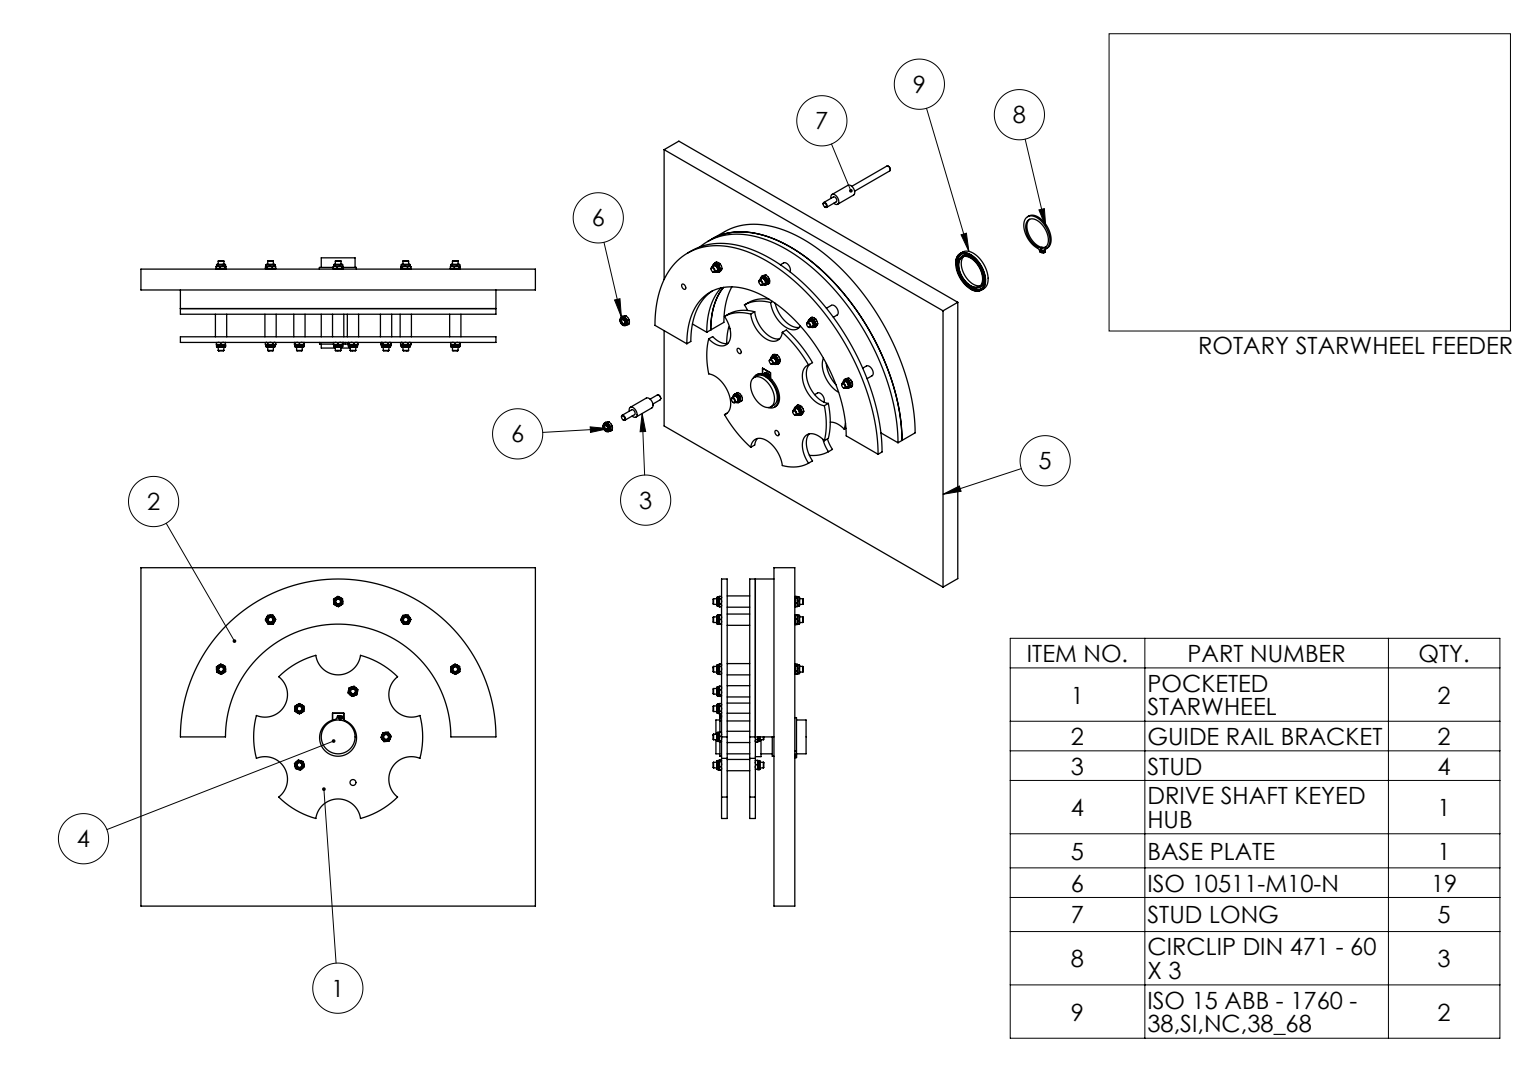
ISO-10303-21;
HEADER;
FILE_DESCRIPTION (('STEP AP214'),
    '1' );
FILE_NAME ('MAS-196',
    '2026-10-23T05:12:30',
    ( '' ),
    ( '' ),
    'SwSTEP 2.0',
    'SolidWorks 2026',
    '' );
FILE_SCHEMA (( 'AUTOMOTIVE_DESIGN' ));
ENDSEC;

DATA;
#1 = LINE ( 'NONE', #2495, #1142 ) ;
#2 = SURFACE_SIDE_STYLE ('',( #1097 ) ) ;
#3 = SURFACE_STYLE_USAGE ( .BOTH. , #3079 ) ;
#4 = AXIS2_PLACEMENT_3D ( 'NONE', #5314, #2448, #2411 ) ;
#5 = CARTESIAN_POINT ( 'NONE',  ( -63.76644452187071721, 49.96174644486006855, -40.00000000000000000 ) ) ;
#6 = PRODUCT ( 'Pocketed Starwheel', 'Pocketed Starwheel', '', ( #881 ) ) ;
#7 = ORIENTED_EDGE ( 'NONE', *, *, #982, .F. ) ;
#8 = EDGE_LOOP ( 'NONE', ( #780, #5698, #1230, #898 ) ) ;
#9 = AXIS2_PLACEMENT_3D ( 'NONE', #5192, #2676, #2095 ) ;
#10 = CARTESIAN_POINT ( 'NONE',  ( 213.0929183184020701, 119.9981648402868331, 10.00000000000000000 ) ) ;
#11 = CARTESIAN_POINT ( 'NONE',  ( 5.459126460941067016, -34.89491303563345070, -3.000000000000000000 ) ) ;
#12 = CIRCLE ( 'NONE', #1262, 6.099504629071905271 ) ;
#13 = CARTESIAN_POINT ( 'NONE',  ( 3.199999999999996181, 4.555686092828153507E-15, 37.19999999999999574 ) ) ;
#14 = ORIENTED_EDGE ( 'NONE', *, *, #6597, .T. ) ;
#15 = ORIENTED_EDGE ( 'NONE', *, *, #7014, .T. ) ;
#16 = AXIS2_PLACEMENT_3D ( 'NONE', #1817, #35, #4883 ) ;
#17 = DIRECTION ( 'NONE',  ( 1.000000000000000000, 0.000000000000000000, 0.000000000000000000 ) ) ;
#18 = CARTESIAN_POINT ( 'NONE',  ( -5.249999999999968026, 239.9963296805737230, 10.00000000000000000 ) ) ;
#19 = FACE_OUTER_BOUND ( 'NONE', #6377, .T. ) ;
#20 = DIRECTION ( 'NONE',  ( -1.000000000000000000, 0.000000000000000000, 0.000000000000000000 ) ) ;
#21 = CARTESIAN_POINT ( 'NONE',  ( -279.9963296805736945, 3.428966089163216048E-14, 0.000000000000000000 ) ) ;
#22 = ORIENTED_EDGE ( 'NONE', *, *, #2120, .F. ) ;
#23 = AXIS2_PLACEMENT_3D ( 'NONE', #6138, #4316, #7358 ) ;
#24 = CARTESIAN_POINT ( 'NONE',  ( 129.9038105676649764, 75.00000000000153477, 10.00000000000000000 ) ) ;
#25 = DIRECTION ( 'NONE',  ( -0.000000000000000000, -0.000000000000000000, 1.000000000000000000 ) ) ;
#26 = DIRECTION ( 'NONE',  ( -0.000000000000000000, -0.000000000000000000, 1.000000000000000000 ) ) ;
#27 = CARTESIAN_POINT ( 'NONE',  ( -7.039801714450301422E-15, 0.000000000000000000, -82.99999999999995737 ) ) ;
#28 = CARTESIAN_POINT ( 'NONE',  ( -58.76644452187068168, 49.96174644486002592, -40.00000000000000000 ) ) ;
#29 = DIRECTION ( 'NONE',  ( -1.000000000000000000, 0.000000000000000000, 0.000000000000000000 ) ) ;
#30 = ORIENTED_EDGE ( 'NONE', *, *, #1780, .F. ) ;
#31 = CIRCLE ( 'NONE', #2437, 40.00000000000001421 ) ;
#32 = EDGE_CURVE ( 'NONE', #3001, #1611, #576, .T. ) ;
#33 = ORIENTED_EDGE ( 'NONE', *, *, #894, .F. ) ;
#34 = ORIENTED_EDGE ( 'NONE', *, *, #1918, .F. ) ;
#35 = DIRECTION ( 'NONE',  ( -0.000000000000000000, -0.000000000000000000, 1.000000000000000000 ) ) ;
#36 =( NAMED_UNIT ( * ) PLANE_ANGLE_UNIT ( ) SI_UNIT ( $, .RADIAN. ) );
#37 = CIRCLE ( 'NONE', #2942, 5.249999999999991118 ) ;
#38 = PRODUCT_DEFINITION_FORMATION_WITH_SPECIFIED_SOURCE ( 'ANY', '', #6, .NOT_KNOWN. ) ;
#39 = DIRECTION ( 'NONE',  ( 1.000000000000000000, 0.000000000000000000, 0.000000000000000000 ) ) ;
#40 = ADVANCED_FACE ( 'NONE', ( #3233 ), #3303, .T. ) ;
#41 = ORIENTED_EDGE ( 'NONE', *, *, #4752, .T. ) ;
#42 = ORIENTED_EDGE ( 'NONE', *, *, #2330, .T. ) ;
#43 = CARTESIAN_POINT ( 'NONE',  ( -68.76644452187024115, -49.96174644486060856, 10.00000000000000000 ) ) ;
#44 = LINE ( 'NONE', #2388, #7655 ) ;
#45 = AXIS2_PLACEMENT_3D ( 'NONE', #3946, #5204, #2688 ) ;
#46 = DIRECTION ( 'NONE',  ( 0.000000000000000000, -1.000000000000000000, 0.000000000000000000 ) ) ;
#47 = VERTEX_POINT ( 'NONE', #965 ) ;
#48 = EDGE_CURVE ( 'NONE', #5972, #47, #4560, .T. ) ;
#49 = ORIENTED_EDGE ( 'NONE', *, *, #2998, .F. ) ;
#50 = COLOUR_RGB ( '',0.8941176470588234615, 0.8941176470588234615, 0.8941176470588234615 ) ;
#51 = DIRECTION ( 'NONE',  ( -0.000000000000000000, -0.000000000000000000, 1.000000000000000000 ) ) ;
#52 = CARTESIAN_POINT ( 'NONE',  ( 0.000000000000000000, 0.000000000000000000, 0.000000000000000000 ) ) ;
#53 = DIRECTION ( 'NONE',  ( 0.000000000000000000, 0.000000000000000000, -1.000000000000000000 ) ) ;
#54 = FACE_BOUND ( 'NONE', #7641, .T. ) ;
#55 = CONTEXT_DEPENDENT_SHAPE_REPRESENTATION ( #2402, #2599 ) ;
#56 = DIRECTION ( 'NONE',  ( 1.000000000000000000, 0.000000000000000000, 0.000000000000000000 ) ) ;
#57 = VERTEX_POINT ( 'NONE', #3381 ) ;
#58 = VECTOR ( 'NONE', #4339, 1000.000000000000000 ) ;
#59 = DIRECTION ( 'NONE',  ( -1.000000000000000000, 0.000000000000000000, 0.000000000000000000 ) ) ;
#60 = CIRCLE ( 'NONE', #2217, 35.25000000000000000 ) ;
#61 = MECHANICAL_DESIGN_GEOMETRIC_PRESENTATION_REPRESENTATION (  '', ( #4091 ), #6487 ) ;
#62 = FACE_BOUND ( 'NONE', #7747, .T. ) ;
#63 = CARTESIAN_POINT ( 'NONE',  ( 1.499999999999999334, -33.63777638310832430, 0.000000000000000000 ) ) ;
#64 = DIRECTION ( 'NONE',  ( -8.771527099359197879E-17, 7.358275397094370797E-17, 0.9999999999999998890 ) ) ;
#65 = PRODUCT_DEFINITION_SHAPE ( 'NONE', 'NONE',  #7795 ) ;
#66 = DIRECTION ( 'NONE',  ( 0.000000000000000000, 0.000000000000000000, -1.000000000000000000 ) ) ;
#67 = DIRECTION ( 'NONE',  ( -0.000000000000000000, 0.000000000000000000, 1.000000000000000000 ) ) ;
#68 = LINE ( 'NONE', #4286, #4450 ) ;
#69 = ORIENTED_EDGE ( 'NONE', *, *, #6641, .F. ) ;
#70 = ORIENTED_EDGE ( 'NONE', *, *, #5383, .T. ) ;
#71 = PRODUCT_RELATED_PRODUCT_CATEGORY ( 'part', '', ( #3721 ) ) ;
#72 = ORIENTED_EDGE ( 'NONE', *, *, #191, .F. ) ;
#73 = AXIS2_PLACEMENT_3D ( 'NONE', #3371, #4109, #6565 ) ;
#74 = CARTESIAN_POINT ( 'NONE',  ( 9.568665290872617746, -28.43309066125681994, -139.9999999999999716 ) ) ;
#75 = SURFACE_STYLE_FILL_AREA ( #3195 ) ;
#76 = SURFACE_STYLE_FILL_AREA ( #5998 ) ;
#77 = DIRECTION ( 'NONE',  ( -0.000000000000000000, -0.000000000000000000, 1.000000000000000000 ) ) ;
#78 = ORIENTED_EDGE ( 'NONE', *, *, #2938, .F. ) ;
#79 = AXIS2_PLACEMENT_3D ( 'NONE', #1466, #7494, #2111 ) ;
#80 = ORIENTED_EDGE ( 'NONE', *, *, #2127, .F. ) ;
#81 = EDGE_CURVE ( 'NONE', #1868, #4093, #1608, .T. ) ;
#82 = EDGE_CURVE ( 'NONE', #2245, #3533, #4731, .T. ) ;
#83 = CYLINDRICAL_SURFACE ( 'NONE', #246, 6.099504629071905271 ) ;
#84 = EDGE_CURVE ( 'NONE', #322, #6002, #3102, .T. ) ;
#85 = LINE ( 'NONE', #6673, #727 ) ;
#86 = CARTESIAN_POINT ( 'NONE',  ( 1.469553684752138043E-14, 239.9963296805737230, 10.00000000000000178 ) ) ;
#87 = EDGE_LOOP ( 'NONE', ( #2176, #4248, #1916, #2842 ) ) ;
#88 = ADVANCED_FACE ( 'NONE', ( #7673 ), #6574, .T. ) ;
#89 = EDGE_LOOP ( 'NONE', ( #7123, #2974, #1891, #2327 ) ) ;
#90 = LINE ( 'NONE', #4231, #2988 ) ;
#91 = DIRECTION ( 'NONE',  ( 0.000000000000000000, 0.000000000000000000, -1.000000000000000000 ) ) ;
#92 = DIRECTION ( 'NONE',  ( 0.000000000000000000, 0.000000000000000000, 1.000000000000000000 ) ) ;
#93 = CARTESIAN_POINT ( 'NONE',  ( 4.586480920263560357, -37.21846574978686562, -3.000000000000000000 ) ) ;
#94 = EDGE_CURVE ( 'NONE', #7689, #4484, #451, .T. ) ;
#95 = VECTOR ( 'NONE', #2161, 1000.000000000000000 ) ;
#96 = CARTESIAN_POINT ( 'NONE',  ( 85.00000000000000000, 9.720002580593245511E-13, 0.000000000000000000 ) ) ;
#97 = ORIENTED_EDGE ( 'NONE', *, *, #4752, .F. ) ;
#98 = AXIS2_PLACEMENT_3D ( 'NONE', #4234, #3767, #1954 ) ;
#99 = DIRECTION ( 'NONE',  ( 0.000000000000000000, 0.000000000000000000, 1.000000000000000000 ) ) ;
#100 = DIRECTION ( 'NONE',  ( 1.000000000000000000, 0.000000000000000000, 0.000000000000000000 ) ) ;
#101 = DIRECTION ( 'NONE',  ( 0.000000000000000000, 0.000000000000000000, 1.000000000000000000 ) ) ;
#102 = DIRECTION ( 'NONE',  ( 0.000000000000000000, 0.000000000000000000, 1.000000000000000000 ) ) ;
#103 = LINE ( 'NONE', #1889, #2646 ) ;
#104 = DIRECTION ( 'NONE',  ( -0.000000000000000000, -0.000000000000000000, 1.000000000000000000 ) ) ;
#105 = CIRCLE ( 'NONE', #7531, 28.50000000000000355 ) ;
#106 = EDGE_LOOP ( 'NONE', ( #1599, #408, #5077, #4129 ) ) ;
#107 = ORIENTED_EDGE ( 'NONE', *, *, #1973, .T. ) ;
#108 = AXIS2_PLACEMENT_3D ( 'NONE', #2705, #5693, #1397 ) ;
#109 = ORIENTED_EDGE ( 'NONE', *, *, #3940, .F. ) ;
#110 = FACE_OUTER_BOUND ( 'NONE', #139, .T. ) ;
#111 = DIRECTION ( 'NONE',  ( -1.000000000000000000, 0.000000000000000000, 0.000000000000000000 ) ) ;
#112 =( NAMED_UNIT ( * ) SI_UNIT ( $, .STERADIAN. ) SOLID_ANGLE_UNIT ( ) );
#113 = DIRECTION ( 'NONE',  ( 0.9412010056177179118, 0.3378471059875997051, 0.000000000000000000 ) ) ;
#114 = CIRCLE ( 'NONE', #2185, 5.250000000000004441 ) ;
#115 = VERTEX_POINT ( 'NONE', #5393 ) ;
#116 = ORIENTED_EDGE ( 'NONE', *, *, #4379, .T. ) ;
#117 =( REPRESENTATION_RELATIONSHIP ('NONE','NONE', #1229, #1433 ) REPRESENTATION_RELATIONSHIP_WITH_TRANSFORMATION ( #7743 )SHAPE_REPRESENTATION_RELATIONSHIP( ) );
#118 = ORIENTED_EDGE ( 'NONE', *, *, #897, .F. ) ;
#119 = CIRCLE ( 'NONE', #3022, 10.00000000000000178 ) ;
#120 = DIRECTION ( 'NONE',  ( -0.000000000000000000, -0.000000000000000000, 1.000000000000000000 ) ) ;
#121 = CARTESIAN_POINT ( 'NONE',  ( -125.2481648402867762, 207.8429183184021554, -8.673617379884035472E-15 ) ) ;
#122 = EDGE_CURVE ( 'NONE', #3301, #4257, #4430, .T. ) ;
#123 = DIRECTION ( 'NONE',  ( 1.000000000000000000, 0.000000000000000000, 0.000000000000000000 ) ) ;
#124 = CARTESIAN_POINT ( 'NONE',  ( 8.000000000000001776, -3.867591403079175372, -4.202324684675417643 ) ) ;
#125 = EDGE_CURVE ( 'NONE', #6200, #406, #1228, .T. ) ;
#126 = EDGE_LOOP ( 'NONE', ( #5453, #5673, #2876, #41 ) ) ;
#127 = COLOUR_RGB ( '',1.000000000000000000, 0.9490196078431372140, 0.9098039215686274384 ) ;
#128 = EDGE_CURVE ( 'NONE', #1948, #4169, #2830, .T. ) ;
#129 = ADVANCED_FACE ( 'NONE', ( #4716 ), #4423, .T. ) ;
#130 = ORIENTED_EDGE ( 'NONE', *, *, #1178, .T. ) ;
#131 = PRODUCT ( 'Drive Shaft Keyed Hub', 'Drive Shaft Keyed Hub', '', ( #3775 ) ) ;
#132 = CARTESIAN_POINT ( 'NONE',  ( -20.63749999999999929, 0.000000000000000000, 0.000000000000000000 ) ) ;
#133 = CARTESIAN_POINT ( 'NONE',  ( -32.81578194438969120, 1.484218055610309728, 0.000000000000000000 ) ) ;
#134 = AXIS2_PLACEMENT_3D ( 'NONE', #2062, #2024, #2612 ) ;
#135 = CARTESIAN_POINT ( 'NONE',  ( 0.000000000000000000, 0.000000000000000000, 10.00000000000000000 ) ) ;
#136 = DIRECTION ( 'NONE',  ( 0.000000000000000000, 0.000000000000000000, 1.000000000000000000 ) ) ;
#137 = LINE ( 'NONE', #2482, #1537 ) ;
#138 = EDGE_CURVE ( 'NONE', #7150, #5807, #1160, .T. ) ;
#139 = EDGE_LOOP ( 'NONE', ( #4956, #6547, #3678, #7659 ) ) ;
#140 = VECTOR ( 'NONE', #2880, 1000.000000000000000 ) ;
#141 = CARTESIAN_POINT ( 'NONE',  ( -39.64284999284935651, -144.6666666666667140, 10.00000000000000000 ) ) ;
#142 = CARTESIAN_POINT ( 'NONE',  ( 8.000000000000000000, 3.871967595402126872, -4.201061386767543482 ) ) ;
#143 = DIRECTION ( 'NONE',  ( -0.000000000000000000, -0.000000000000000000, 1.000000000000000000 ) ) ;
#144 = FACE_OUTER_BOUND ( 'NONE', #3867, .T. ) ;
#145 = DIRECTION ( 'NONE',  ( 1.000000000000000000, 0.000000000000000000, 0.000000000000000000 ) ) ;
#146 = CARTESIAN_POINT ( 'NONE',  ( 105.4635834177229299, 106.6650485055578770, 0.000000000000000000 ) ) ;
#147 = VERTEX_POINT ( 'NONE', #4043 ) ;
#148 = EDGE_LOOP ( 'NONE', ( #2715, #5380, #1534, #3342 ) ) ;
#149 = ORIENTED_EDGE ( 'NONE', *, *, #2680, .T. ) ;
#150 = DIRECTION ( 'NONE',  ( 0.9938725510941108787, -0.1105321318969463978, 0.000000000000000000 ) ) ;
#151 = CARTESIAN_POINT ( 'NONE',  ( -5.459126460941067016, -34.89491303563345070, 0.000000000000000000 ) ) ;
#152 = CARTESIAN_POINT ( 'NONE',  ( 0.3344772040064616925, 0.000000000000000000, 31.52499999999999858 ) ) ;
#153 = CIRCLE ( 'NONE', #6952, 37.50000000000000000 ) ;
#154 = VERTEX_POINT ( 'NONE', #7084 ) ;
#155 = ORIENTED_EDGE ( 'NONE', *, *, #176, .F. ) ;
#156 = ORIENTED_EDGE ( 'NONE', *, *, #2886, .T. ) ;
#157 = VECTOR ( 'NONE', #4793, 1000.000000000000000 ) ;
#158 = AXIS2_PLACEMENT_3D ( 'NONE', #3282, #2691, #5085 ) ;
#159 = EDGE_CURVE ( 'NONE', #1610, #2529, #7077, .T. ) ;
#160 = DIRECTION ( 'NONE',  ( 1.000000000000000000, 0.000000000000000000, 0.000000000000000000 ) ) ;
#161 = SURFACE_STYLE_FILL_AREA ( #749 ) ;
#162 = DIRECTION ( 'NONE',  ( -0.000000000000000000, -0.000000000000000000, 1.000000000000000000 ) ) ;
#163 = DIRECTION ( 'NONE',  ( 1.000000000000000000, 0.000000000000000000, 0.000000000000000000 ) ) ;
#164 = AXIS2_PLACEMENT_3D ( 'NONE', #7366, #2525, #6697 ) ;
#165 = ORIENTED_EDGE ( 'NONE', *, *, #3978, .F. ) ;
#166 = DIRECTION ( 'NONE',  ( -1.000000000000000000, 0.000000000000000000, 0.000000000000000000 ) ) ;
#167 = DIRECTION ( 'NONE',  ( 0.000000000000000000, 0.000000000000000000, 1.000000000000000000 ) ) ;
#168 = CIRCLE ( 'NONE', #5710, 4.171999999999995268 ) ;
#169 = DIRECTION ( 'NONE',  ( 1.000000000000000000, 0.000000000000000000, 0.000000000000000000 ) ) ;
#170 = ADVANCED_FACE ( 'NONE', ( #5231 ), #1395, .T. ) ;
#171 = LINE ( 'NONE', #6767, #1288 ) ;
#172 = ORIENTED_EDGE ( 'NONE', *, *, #2324, .T. ) ;
#173 = AXIS2_PLACEMENT_3D ( 'NONE', #1594, #994, #5732 ) ;
#174 = DIRECTION ( 'NONE',  ( -0.8660254037844382635, -0.5000000000000005551, 0.000000000000000000 ) ) ;
#175 = DIRECTION ( 'NONE',  ( -1.000000000000000000, 0.000000000000000000, 0.000000000000000000 ) ) ;
#176 = EDGE_CURVE ( 'NONE', #406, #5752, #7525, .T. ) ;
#177 = CARTESIAN_POINT ( 'NONE',  ( 8.000000000000000000, 4.618802153517013842, -3.985468820183668104 ) ) ;
#178 = LINE ( 'NONE', #6692, #6392 ) ;
#179 = DIRECTION ( 'NONE',  ( 0.9135454576426065287, -0.4067366430757879958, 0.000000000000000000 ) ) ;
#180 = STYLED_ITEM ( 'NONE', ( #6391 ), #5011 ) ;
#181 = ADVANCED_FACE ( 'NONE', ( #7711 ), #4121, .F. ) ;
#182 = FACE_OUTER_BOUND ( 'NONE', #3425, .T. ) ;
#183 = CARTESIAN_POINT ( 'NONE',  ( 0.000000000000000000, 0.000000000000000000, -4.700000000000000178 ) ) ;
#184 = ORIENTED_EDGE ( 'NONE', *, *, #6782, .F. ) ;
#185 = VERTEX_POINT ( 'NONE', #2518 ) ;
#186 = AXIS2_PLACEMENT_3D ( 'NONE', #4038, #490, #7002 ) ;
#187 = ADVANCED_FACE ( 'NONE', ( #728, #6616 ), #2484, .T. ) ;
#188 = ORIENTED_EDGE ( 'NONE', *, *, #6602, .F. ) ;
#189 = CYLINDRICAL_SURFACE ( 'NONE', #7328, 5.000000000000004441 ) ;
#190 = DIRECTION ( 'NONE',  ( 0.000000000000000000, -0.000000000000000000, -1.000000000000000000 ) ) ;
#191 = EDGE_CURVE ( 'NONE', #6189, #4002, #7244, .T. ) ;
#192 = AXIS2_PLACEMENT_3D ( 'NONE', #4761, #4244, #2487 ) ;
#193 = PRODUCT_DEFINITION_SHAPE ( 'NONE', 'NONE',  #7770 ) ;
#194 = VERTEX_POINT ( 'NONE', #3652 ) ;
#195 = ORIENTED_EDGE ( 'NONE', *, *, #3698, .F. ) ;
#196 = CARTESIAN_POINT ( 'NONE',  ( -0.5700000000000001732, -28.49429942988597020, -3.000000000000000000 ) ) ;
#197 = CARTESIAN_POINT ( 'NONE',  ( -5.554394503829287011, 27.95350964898380752, -79.99999999999995737 ) ) ;
#198 = AXIS2_PLACEMENT_3D ( 'NONE', #1671, #7152, #4070 ) ;
#199 = CARTESIAN_POINT ( 'NONE',  ( -20.63749999999999574, 0.000000000000000000, 0.000000000000000000 ) ) ;
#200 = EDGE_LOOP ( 'NONE', ( #6714, #643, #5819, #2337 ) ) ;
#201 = DIRECTION ( 'NONE',  ( -2.403401228516536951E-14, -1.000000000000000000, 0.000000000000000000 ) ) ;
#202 = DIRECTION ( 'NONE',  ( 1.000000000000000000, 0.000000000000000000, 0.000000000000000000 ) ) ;
#203 = CARTESIAN_POINT ( 'NONE',  ( 9.090232026328989079, -27.01143612819398143, -119.9999999999999716 ) ) ;
#204 = ITEM_DEFINED_TRANSFORMATION ( 'NONE', 'NONE', #2809,  #7485 ) ;
#205 = CARTESIAN_POINT ( 'NONE',  ( 9.090232026328989079, -27.01143612819398143, -122.9999999999999716 ) ) ;
#206 = EDGE_LOOP ( 'NONE', ( #7630, #2753 ) ) ;
#207 = AXIS2_PLACEMENT_3D ( 'NONE', #2317, #4702, #7112 ) ;
#208 = FACE_OUTER_BOUND ( 'NONE', #6661, .T. ) ;
#209 = DIRECTION ( 'NONE',  ( 1.000000000000000000, 0.000000000000000000, 0.000000000000000000 ) ) ;
#210 = AXIS2_PLACEMENT_3D ( 'NONE', #7506, #2784, #5179 ) ;
#211 = CARTESIAN_POINT ( 'NONE',  ( 8.000000000000000000, 4.618802153517004072, -4.700000000000000178 ) ) ;
#212 = DIRECTION ( 'NONE',  ( -0.000000000000000000, -0.000000000000000000, -1.000000000000000000 ) ) ;
#213 = CARTESIAN_POINT ( 'NONE',  ( 119.9981648402867194, 207.8429183184022691, 14.70000000000000462 ) ) ;
#214 = CARTESIAN_POINT ( 'NONE',  ( 5.777789833161707559E-31, -4.119912841284263785E-15, -119.9999999999999716 ) ) ;
#215 = EDGE_CURVE ( 'NONE', #5454, #5308, #3730, .T. ) ;
#216 = CARTESIAN_POINT ( 'NONE',  ( 4.000000000000000000, -33.63777638310832430, -3.000000000000000000 ) ) ;
#217 = ORIENTED_EDGE ( 'NONE', *, *, #263, .T. ) ;
#218 = EDGE_CURVE ( 'NONE', #491, #1814, #4911, .T. ) ;
#219 = VERTEX_POINT ( 'NONE', #3065 ) ;
#220 = ADVANCED_FACE ( 'NONE', ( #4830 ), #7323, .F. ) ;
#221 = CIRCLE ( 'NONE', #3133, 5.250000000000004441 ) ;
#222 = ORIENTED_EDGE ( 'NONE', *, *, #6161, .T. ) ;
#223 = EDGE_CURVE ( 'NONE', #6783, #3903, #7702, .T. ) ;
#224 = DIRECTION ( 'NONE',  ( 0.000000000000000000, 0.000000000000000000, -1.000000000000000000 ) ) ;
#225 = DIRECTION ( 'NONE',  ( -0.5000000000000006661, -0.8660254037844383745, 0.000000000000000000 ) ) ;
#226 = CARTESIAN_POINT ( 'NONE',  ( -28.05900627794857627, -4.994213320838723824, -79.99999999999995737 ) ) ;
#227 = VECTOR ( 'NONE', #3090, 1000.000000000000000 ) ;
#228 = DIRECTION ( 'NONE',  ( 0.000000000000000000, 0.000000000000000000, -1.000000000000000000 ) ) ;
#229 = ADVANCED_FACE ( 'NONE', ( #767 ), #4425, .T. ) ;
#230 = ORIENTED_EDGE ( 'NONE', *, *, #4072, .F. ) ;
#231 = VECTOR ( 'NONE', #6497, 1000.000000000000114 ) ;
#232 = ORIENTED_EDGE ( 'NONE', *, *, #991, .T. ) ;
#233 = DIRECTION ( 'NONE',  ( -1.000000000000000000, 0.000000000000000000, 0.000000000000000000 ) ) ;
#234 = VECTOR ( 'NONE', #92, 1000.000000000000000 ) ;
#235 = CARTESIAN_POINT ( 'NONE',  ( -3.200000000000007727, 0.000000000000000000, 0.000000000000000000 ) ) ;
#236 = CARTESIAN_POINT ( 'NONE',  ( 4.000000000000005329, -6.928203230275506108, 0.000000000000000000 ) ) ;
#237 = ORIENTED_EDGE ( 'NONE', *, *, #4138, .F. ) ;
#238 = CONICAL_SURFACE ( 'NONE', #4018, 8.000000000000000000, 1.047197551196596299 ) ;
#239 = LINE ( 'NONE', #274, #7501 ) ;
#240 = DIRECTION ( 'NONE',  ( -0.000000000000000000, -0.000000000000000000, -1.000000000000000000 ) ) ;
#241 = CARTESIAN_POINT ( 'NONE',  ( -1.313474075707227406, -8.479269695850861766, -4.383279549040158152 ) ) ;
#242 = CIRCLE ( 'NONE', #872, 0.7500000000000041078 ) ;
#243 = LINE ( 'NONE', #4981, #3185 ) ;
#244 = EDGE_LOOP ( 'NONE', ( #4274, #4627, #3628, #1463, #5044, #4969, #332, #6418, #2566, #3083, #602, #296, #1781, #3453, #237, #2234 ) ) ;
#245 = CARTESIAN_POINT ( 'NONE',  ( 207.8429183184021269, 119.9981648402868331, -50.00000000000000000 ) ) ;
#246 = AXIS2_PLACEMENT_3D ( 'NONE', #7304, #4299, #6708 ) ;
#247 = DIRECTION ( 'NONE',  ( -1.000000000000000000, 0.000000000000000000, 0.000000000000000000 ) ) ;
#248 = DIRECTION ( 'NONE',  ( -1.000000000000000000, 0.000000000000000000, 0.000000000000000000 ) ) ;
#249 = DIRECTION ( 'NONE',  ( -0.09063257223759993431, -0.9958843993404034034, 0.000000000000000000 ) ) ;
#250 = APPLICATION_PROTOCOL_DEFINITION ( 'draft international standard', 'automotive_design', 1998, #2547 ) ;
#251 = PRODUCT_DEFINITION_SHAPE ( 'NONE', 'NONE',  #7775 ) ;
#252 = CYLINDRICAL_SURFACE ( 'NONE', #6988, 29.99999999999999289 ) ;
#253 = FACE_OUTER_BOUND ( 'NONE', #5709, .T. ) ;
#254 = ORIENTED_EDGE ( 'NONE', *, *, #7228, .T. ) ;
#255 = ORIENTED_EDGE ( 'NONE', *, *, #5004, .T. ) ;
#256 = VERTEX_POINT ( 'NONE', #1883 ) ;
#257 = VERTEX_POINT ( 'NONE', #4355 ) ;
#258 = AXIS2_PLACEMENT_3D ( 'NONE', #3304, #337, #5703 ) ;
#259 = DIRECTION ( 'NONE',  ( -0.000000000000000000, -0.000000000000000000, 1.000000000000000000 ) ) ;
#260 = DIRECTION ( 'NONE',  ( 0.000000000000000000, 0.000000000000000000, -1.000000000000000000 ) ) ;
#261 = SHAPE_DEFINITION_REPRESENTATION ( #5042, #1229 ) ;
#262 = CARTESIAN_POINT ( 'NONE',  ( -68.76644452187068168, 49.96174644486002592, 0.000000000000000000 ) ) ;
#263 = EDGE_CURVE ( 'NONE', #257, #1814, #3618, .T. ) ;
#264 = ORIENTED_EDGE ( 'NONE', *, *, #3362, .F. ) ;
#265 = ORIENTED_EDGE ( 'NONE', *, *, #789, .F. ) ;
#266 = ORIENTED_EDGE ( 'NONE', *, *, #6459, .F. ) ;
#267 = CARTESIAN_POINT ( 'NONE',  ( 0.000000000000000000, 0.000000000000000000, -139.9999999999999716 ) ) ;
#268 = EDGE_CURVE ( 'NONE', #736, #6870, #4277, .T. ) ;
#269 = FACE_OUTER_BOUND ( 'NONE', #4910, .T. ) ;
#270 = CARTESIAN_POINT ( 'NONE',  ( 10.00000000000000000, 41.99999999999999289, -60.00000000000000711 ) ) ;
#271 = DIRECTION ( 'NONE',  ( 0.000000000000000000, 0.000000000000000000, 1.000000000000000000 ) ) ;
#272 = ORIENTED_EDGE ( 'NONE', *, *, #7163, .T. ) ;
#273 = CIRCLE ( 'NONE', #5186, 30.30000000000000071 ) ;
#274 = CARTESIAN_POINT ( 'NONE',  ( 10.00000000000000000, 42.00000000000000000, 0.000000000000000000 ) ) ;
#275 = LINE ( 'NONE', #5724, #2339 ) ;
#276 = DIRECTION ( 'NONE',  ( 1.000000000000000000, 0.000000000000000000, 0.000000000000000000 ) ) ;
#277 = AXIS2_PLACEMENT_3D ( 'NONE', #4146, #677, #1148 ) ;
#278 = ORIENTED_EDGE ( 'NONE', *, *, #4857, .T. ) ;
#279 = FACE_OUTER_BOUND ( 'NONE', #4266, .T. ) ;
#280 = EDGE_CURVE ( 'NONE', #719, #2423, #3235, .T. ) ;
#281 = ORIENTED_EDGE ( 'NONE', *, *, #3745, .T. ) ;
#282 = CARTESIAN_POINT ( 'NONE',  ( -72.93844452187067873, 49.96174644486002592, 25.00000000000000000 ) ) ;
#283 = TOROIDAL_SURFACE ( 'NONE', #2189, 37.19999999999999574, 0.3000000000000007661 ) ;
#284 = CARTESIAN_POINT ( 'NONE',  ( 0.000000000000000000, 0.000000000000000000, -122.9999999999999716 ) ) ;
#285 = CARTESIAN_POINT ( 'NONE',  ( -207.8429183184020985, 119.9981648402869467, 10.00000000000000178 ) ) ;
#286 = DIRECTION ( 'NONE',  ( -0.000000000000000000, -0.000000000000000000, 1.000000000000000000 ) ) ;
#287 = CARTESIAN_POINT ( 'NONE',  ( 0.000000000000000000, 0.000000000000000000, -60.00000000000000000 ) ) ;
#288 = ITEM_DEFINED_TRANSFORMATION ( 'NONE', 'NONE', #941,  #7485 ) ;
#289 = DIRECTION ( 'NONE',  ( 0.000000000000000000, 0.000000000000000000, 1.000000000000000000 ) ) ;
#290 = AXIS2_PLACEMENT_3D ( 'NONE', #4924, #77, #3632 ) ;
#291 = ORIENTED_EDGE ( 'NONE', *, *, #5808, .T. ) ;
#292 = EDGE_LOOP ( 'NONE', ( #3015, #4779, #3543, #2009 ) ) ;
#293 = VERTEX_POINT ( 'NONE', #6097 ) ;
#294 = VERTEX_POINT ( 'NONE', #141 ) ;
#295 = B_SPLINE_CURVE_WITH_KNOTS ( 'NONE', 3,
 ( #3128, #6526, #3715, #4929, #3487, #4111 ),
 .UNSPECIFIED., .F., .F.,
 ( 4, 2, 4 ),
 ( 0.008240550023493524098, 0.01057684187039405026, 0.01291313371729457642 ),
 .UNSPECIFIED. ) ;
#296 = ORIENTED_EDGE ( 'NONE', *, *, #5918, .F. ) ;
#297 = AXIS2_PLACEMENT_3D ( 'NONE', #3501, #3421, #499 ) ;
#298 = CIRCLE ( 'NONE', #1308, 5.249999999999976907 ) ;
#299 = CARTESIAN_POINT ( 'NONE',  ( -10.00000000000000000, 28.28427124746189136, -50.00000000000000000 ) ) ;
#300 = CARTESIAN_POINT ( 'NONE',  ( -8.000000000000000000, 1.572549600175615625, -0.06894455525513183691 ) ) ;
#301 = DIRECTION ( 'NONE',  ( 0.9412010056177179118, 0.3378471059875997051, 0.000000000000000000 ) ) ;
#302 = PRODUCT_DEFINITION ( 'UNKNOWN', '', #6087, #1721 ) ;
#303 = VECTOR ( 'NONE', #4360, 1000.000000000000000 ) ;
#304 = ORIENTED_EDGE ( 'NONE', *, *, #4363, .T. ) ;
#305 = PRESENTATION_LAYER_ASSIGNMENT (  '', '', ( #5849 ) ) ;
#306 = ORIENTED_EDGE ( 'NONE', *, *, #3124, .T. ) ;
#307 = ORIENTED_EDGE ( 'NONE', *, *, #7076, .T. ) ;
#308 = DIRECTION ( 'NONE',  ( -0.000000000000000000, -0.000000000000000000, -1.000000000000000000 ) ) ;
#309 =( GEOMETRIC_REPRESENTATION_CONTEXT ( 3 ) GLOBAL_UNCERTAINTY_ASSIGNED_CONTEXT ( ( #1741 ) ) GLOBAL_UNIT_ASSIGNED_CONTEXT ( ( #1216, #1786, #4884 ) ) REPRESENTATION_CONTEXT ( 'NONE', 'WORKASPACE' ) );
#310 = CARTESIAN_POINT ( 'NONE',  ( 5.459126460941064352, -34.89491303563345070, 0.000000000000000000 ) ) ;
#311 = CARTESIAN_POINT ( 'NONE',  ( 202.5929183184021269, 119.9981648402868331, 10.00000000000000000 ) ) ;
#312 = EDGE_CURVE ( 'NONE', #3677, #520, #3029, .T. ) ;
#313 = ORIENTED_EDGE ( 'NONE', *, *, #3930, .F. ) ;
#314 = EDGE_CURVE ( 'NONE', #5791, #5558, #448, .T. ) ;
#315 = EDGE_CURVE ( 'NONE', #1373, #3431, #4733, .T. ) ;
#316 = EDGE_CURVE ( 'NONE', #3677, #1170, #2354, .T. ) ;
#317 = PLANE ( 'NONE',  #5373 ) ;
#318 = CARTESIAN_POINT ( 'NONE',  ( -68.76644452187068168, 49.96174644486002592, 24.17200000000001125 ) ) ;
#319 = CIRCLE ( 'NONE', #5110, 29.99999999999999289 ) ;
#320 = CARTESIAN_POINT ( 'NONE',  ( -68.76644452187068168, 49.96174644486002592, 24.17200000000001125 ) ) ;
#321 = DIRECTION ( 'NONE',  ( 1.000000000000000000, 0.000000000000000000, 0.000000000000000000 ) ) ;
#322 = VERTEX_POINT ( 'NONE', #3771 ) ;
#323 = EDGE_CURVE ( 'NONE', #1642, #5517, #7754, .T. ) ;
#324 = AXIS2_PLACEMENT_3D ( 'NONE', #2355, #6089, #6606 ) ;
#325 = FACE_BOUND ( 'NONE', #6779, .T. ) ;
#326 = DIRECTION ( 'NONE',  ( -1.000000000000000000, 1.224646799147352961E-16, 0.000000000000000000 ) ) ;
#327 = EDGE_CURVE ( 'NONE', #2220, #7617, #7205, .T. ) ;
#328 = DIRECTION ( 'NONE',  ( 0.000000000000000000, 0.000000000000000000, 1.000000000000000000 ) ) ;
#329 = LINE ( 'NONE', #3997, #6288 ) ;
#330 = FACE_OUTER_BOUND ( 'NONE', #2807, .T. ) ;
#331 = CARTESIAN_POINT ( 'NONE',  ( 0.000000000000000000, 0.000000000000000000, 0.000000000000000000 ) ) ;
#332 = ORIENTED_EDGE ( 'NONE', *, *, #4857, .F. ) ;
#333 = ORIENTED_EDGE ( 'NONE', *, *, #3563, .F. ) ;
#334 = ORIENTED_EDGE ( 'NONE', *, *, #2127, .T. ) ;
#335 = ORIENTED_EDGE ( 'NONE', *, *, #1569, .F. ) ;
#336 = DIRECTION ( 'NONE',  ( 1.000000000000000000, 0.000000000000000000, 0.000000000000000000 ) ) ;
#337 = DIRECTION ( 'NONE',  ( 0.000000000000000000, 0.000000000000000000, 1.000000000000000000 ) ) ;
#338 = CARTESIAN_POINT ( 'NONE',  ( -8.000000000000000000, 4.618802153517003184, -0.7145311798163286321 ) ) ;
#339 = SURFACE_STYLE_USAGE ( .BOTH. , #6499 ) ;
#340 = CARTESIAN_POINT ( 'NONE',  ( 0.000000000000000000, 0.000000000000000000, 0.000000000000000000 ) ) ;
#341 = CIRCLE ( 'NONE', #4254, 29.99999999999999289 ) ;
#342 = ORIENTED_EDGE ( 'NONE', *, *, #1344, .T. ) ;
#343 = ORIENTED_EDGE ( 'NONE', *, *, #565, .F. ) ;
#344 = ORIENTED_EDGE ( 'NONE', *, *, #1290, .F. ) ;
#345 = AXIS2_PLACEMENT_3D ( 'NONE', #357, #4696, #2348 ) ;
#346 = DIRECTION ( 'NONE',  ( 1.000000000000000000, 0.000000000000000000, 0.000000000000000000 ) ) ;
#347 =( LENGTH_UNIT ( ) NAMED_UNIT ( * ) SI_UNIT ( .MILLI., .METRE. ) );
#348 = FACE_OUTER_BOUND ( 'NONE', #4201, .T. ) ;
#349 = CARTESIAN_POINT ( 'NONE',  ( 28.05900627794855851, 4.994213320838720271, -82.99999999999995737 ) ) ;
#350 = ORIENTED_EDGE ( 'NONE', *, *, #2657, .F. ) ;
#351 = CIRCLE ( 'NONE', #3314, 2.250000000000001776 ) ;
#352 = ORIENTED_EDGE ( 'NONE', *, *, #4240, .F. ) ;
#353 = CIRCLE ( 'NONE', #4261, 29.99999999999999289 ) ;
#354 = EDGE_CURVE ( 'NONE', #6826, #2635, #830, .T. ) ;
#355 = CYLINDRICAL_SURFACE ( 'NONE', #1081, 0.7500000000000041078 ) ;
#356 = CARTESIAN_POINT ( 'NONE',  ( -20.63749999999999929, 0.000000000000000000, 0.000000000000000000 ) ) ;
#357 = CARTESIAN_POINT ( 'NONE',  ( 129.9038105676665396, -74.99999999999882050, 10.00000000000000000 ) ) ;
#358 = ADVANCED_FACE ( 'NONE', ( #4393 ), #7469, .F. ) ;
#359 = CARTESIAN_POINT ( 'NONE',  ( -4.250000000000000000, 5.204748896376250699E-16, 2.573333333332999739 ) ) ;
#360 = ORIENTED_EDGE ( 'NONE', *, *, #6201, .F. ) ;
#361 = AXIS2_PLACEMENT_3D ( 'NONE', #4667, #4589, #6527 ) ;
#362 = EDGE_CURVE ( 'NONE', #3787, #4597, #6330, .T. ) ;
#363 =( REPRESENTATION_RELATIONSHIP ('NONE','NONE', #1229, #1433 ) REPRESENTATION_RELATIONSHIP_WITH_TRANSFORMATION ( #7001 )SHAPE_REPRESENTATION_RELATIONSHIP( ) );
#364 = CARTESIAN_POINT ( 'NONE',  ( -10.00000000000000000, 28.28427124746190202, 0.000000000000000000 ) ) ;
#365 = SURFACE_STYLE_USAGE ( .BOTH. , #7704 ) ;
#366 = DIRECTION ( 'NONE',  ( 1.000000000000000000, 0.000000000000000000, 0.000000000000000000 ) ) ;
#367 = DIRECTION ( 'NONE',  ( -1.000000000000000000, 0.000000000000000000, -0.000000000000000000 ) ) ;
#368 = DIRECTION ( 'NONE',  ( -1.000000000000000000, 0.000000000000000000, 0.000000000000000000 ) ) ;
#369 = EDGE_CURVE ( 'NONE', #2537, #7447, #319, .T. ) ;
#370 = FACE_OUTER_BOUND ( 'NONE', #7061, .T. ) ;
#371 = VERTEX_POINT ( 'NONE', #5060 ) ;
#372 = EDGE_LOOP ( 'NONE', ( #1862, #4014 ) ) ;
#373 = VECTOR ( 'NONE', #6743, 1000.000000000000000 ) ;
#374 = EDGE_LOOP ( 'NONE', ( #679, #6781, #2050, #5404 ) ) ;
#375 = CARTESIAN_POINT ( 'NONE',  ( 4.000000000000004441, 6.928203230275507885, -4.700000000000000178 ) ) ;
#376 = LINE ( 'NONE', #524, #671 ) ;
#377 = CARTESIAN_POINT ( 'NONE',  ( 199.9963296805737230, -4.796075449120964792E-12, -50.00000000000004263 ) ) ;
#378 = CARTESIAN_POINT ( 'NONE',  ( -279.9963296805736945, 3.428966089163216048E-14, 10.00000000000000000 ) ) ;
#379 = AXIS2_PLACEMENT_3D ( 'NONE', #3051, #1902, #6121 ) ;
#380 = VERTEX_POINT ( 'NONE', #1396 ) ;
#381 = ORIENTED_EDGE ( 'NONE', *, *, #6740, .T. ) ;
#382 = AXIS2_PLACEMENT_3D ( 'NONE', #2843, #7643, #5876 ) ;
#383 = ORIENTED_EDGE ( 'NONE', *, *, #6065, .F. ) ;
#384 = DIRECTION ( 'NONE',  ( -0.000000000000000000, -0.000000000000000000, 1.000000000000000000 ) ) ;
#385 = DIRECTION ( 'NONE',  ( -1.000000000000000000, 0.000000000000000000, 0.000000000000000000 ) ) ;
#386 = CARTESIAN_POINT ( 'NONE',  ( 0.000000000000000000, 0.000000000000000000, 0.000000000000000000 ) ) ;
#387 = VERTEX_POINT ( 'NONE', #5026 ) ;
#388 = DIRECTION ( 'NONE',  ( 0.000000000000000000, -1.000000000000000000, 0.000000000000000000 ) ) ;
#389 = DIRECTION ( 'NONE',  ( -0.000000000000000000, -0.000000000000000000, 1.000000000000000000 ) ) ;
#390 = LINE ( 'NONE', #2812, #6033 ) ;
#391 = DIRECTION ( 'NONE',  ( -1.000000000000000000, 0.000000000000000000, 0.000000000000000000 ) ) ;
#392 = CIRCLE ( 'NONE', #1408, 10.00000000000000178 ) ;
#393 = ORIENTED_EDGE ( 'NONE', *, *, #5918, .T. ) ;
#394 = EDGE_CURVE ( 'NONE', #2888, #7603, #5583, .T. ) ;
#395 = DIRECTION ( 'NONE',  ( 0.000000000000000000, 0.000000000000000000, -1.000000000000000000 ) ) ;
#396 =( NAMED_UNIT ( * ) PLANE_ANGLE_UNIT ( ) SI_UNIT ( $, .RADIAN. ) );
#397 = AXIS2_PLACEMENT_3D ( 'NONE', #1905, #4302, #3091 ) ;
#398 = DIRECTION ( 'NONE',  ( 1.000000000000000000, 0.000000000000000000, 0.000000000000000000 ) ) ;
#399 = ADVANCED_FACE ( 'NONE', ( #917 ), #3849, .F. ) ;
#400 = EDGE_CURVE ( 'NONE', #6073, #6532, #1763, .T. ) ;
#401 = CARTESIAN_POINT ( 'NONE',  ( 0.000000000000000000, 4.133182947122317561E-15, -33.75000000000000000 ) ) ;
#402 = CARTESIAN_POINT ( 'NONE',  ( -68.76644452187024115, -49.96174644486060856, 0.000000000000000000 ) ) ;
#403 = DIRECTION ( 'NONE',  ( -1.000000000000000000, 0.000000000000000000, 0.000000000000000000 ) ) ;
#404 = ORIENTED_EDGE ( 'NONE', *, *, #2745, .T. ) ;
#405 = APPLICATION_CONTEXT ( 'automotive_design' ) ;
#406 = VERTEX_POINT ( 'NONE', #4546 ) ;
#407 = CIRCLE ( 'NONE', #7096, 5.250000000000004441 ) ;
#408 = ORIENTED_EDGE ( 'NONE', *, *, #3368, .T. ) ;
#409 = ADVANCED_FACE ( 'NONE', ( #5620 ), #3809, .T. ) ;
#410 = CARTESIAN_POINT ( 'NONE',  ( -5.354491962338127742, 6.146186931204406179, -0.06809871960542698832 ) ) ;
#411 = EDGE_CURVE ( 'NONE', #2919, #6189, #1551, .T. ) ;
#412 = CARTESIAN_POINT ( 'NONE',  ( 5.355005115540895311, 6.145890662064654286, -0.08224679563971268315 ) ) ;
#413 = CARTESIAN_POINT ( 'NONE',  ( -279.9963296805736945, 3.428966089163216048E-14, 576.0908266162076643 ) ) ;
#414 = CARTESIAN_POINT ( 'NONE',  ( 0.000000000000000000, 0.000000000000000000, 0.000000000000000000 ) ) ;
#415 = AXIS2_PLACEMENT_3D ( 'NONE', #6467, #428, #4730 ) ;
#416 = DIRECTION ( 'NONE',  ( -0.000000000000000000, -0.000000000000000000, 1.000000000000000000 ) ) ;
#417 = DIRECTION ( 'NONE',  ( 0.000000000000000000, 0.000000000000000000, 1.000000000000000000 ) ) ;
#418 = ORIENTED_EDGE ( 'NONE', *, *, #2868, .T. ) ;
#419 = EDGE_CURVE ( 'NONE', #4484, #2866, #6124, .T. ) ;
#420 = SHAPE_REPRESENTATION ( 'angular contact ball bearing_68_iso_ISO 15 ABB - 1760 - 38,SI,NC,38_68', ( #7485 ), #6116 ) ;
#421 = VERTEX_POINT ( 'NONE', #3959 ) ;
#422 = VECTOR ( 'NONE', #416, 1000.000000000000000 ) ;
#423 = AXIS2_PLACEMENT_3D ( 'NONE', #6991, #7495, #3952 ) ;
#424 = ORIENTED_EDGE ( 'NONE', *, *, #5929, .F. ) ;
#425 = CARTESIAN_POINT ( 'NONE',  ( 119.9981648402868899, 207.8429183184021269, 10.00000000000000000 ) ) ;
#426 = EDGE_CURVE ( 'NONE', #1610, #4116, #5242, .T. ) ;
#427 = FILL_AREA_STYLE ('',( #1657 ) ) ;
#428 = DIRECTION ( 'NONE',  ( 3.081487911019577365E-33, -2.775557561562891967E-17, -1.000000000000000000 ) ) ;
#429=STYLED_ITEM('',(#7837),#5821);
#430 = DIRECTION ( 'NONE',  ( 1.000000000000000000, 0.000000000000000000, 0.000000000000000000 ) ) ;
#431 = ORIENTED_EDGE ( 'NONE', *, *, #935, .T. ) ;
#432 = ORIENTED_EDGE ( 'NONE', *, *, #905, .T. ) ;
#433 = CONICAL_SURFACE ( 'NONE', #5480, 37.49999999999997868, 1.029744258676654090 ) ;
#434 = FACE_OUTER_BOUND ( 'NONE', #851, .T. ) ;
#435 = CARTESIAN_POINT ( 'NONE',  ( 0.3344772040064616925, 0.000000000000000000, 0.000000000000000000 ) ) ;
#436 = DIRECTION ( 'NONE',  ( 0.7071067811865504593, 8.659560562354968603E-17, -0.7071067811865445751 ) ) ;
#437 = CARTESIAN_POINT ( 'NONE',  ( 0.000000000000000000, 0.000000000000000000, 10.00000000000000000 ) ) ;
#438 = ORIENTED_EDGE ( 'NONE', *, *, #7182, .T. ) ;
#439 = AXIS2_PLACEMENT_3D ( 'NONE', #4678, #3500, #1686 ) ;
#440 = ORIENTED_EDGE ( 'NONE', *, *, #2302, .F. ) ;
#441 = CARTESIAN_POINT ( 'NONE',  ( 0.000000000000000000, 0.000000000000000000, -112.9999999999999716 ) ) ;
#442 = DIRECTION ( 'NONE',  ( 0.000000000000000000, 0.000000000000000000, 1.000000000000000000 ) ) ;
#443 = DIRECTION ( 'NONE',  ( 1.000000000000000000, 0.000000000000000000, -0.000000000000000000 ) ) ;
#444 = FACE_OUTER_BOUND ( 'NONE', #7719, .T. ) ;
#445 = ITEM_DEFINED_TRANSFORMATION ( 'NONE', 'NONE', #4851,  #7485 ) ;
#446 = DIRECTION ( 'NONE',  ( 1.000000000000000000, 0.000000000000000000, 0.000000000000000000 ) ) ;
#447 = ORIENTED_EDGE ( 'NONE', *, *, #323, .F. ) ;
#448 = CIRCLE ( 'NONE', #4230, 40.00000000000000711 ) ;
#449 = ORIENTED_EDGE ( 'NONE', *, *, #7450, .F. ) ;
#450 = ORIENTED_EDGE ( 'NONE', *, *, #4469, .T. ) ;
#451 = LINE ( 'NONE', #5901, #5864 ) ;
#452 = AXIS2_PLACEMENT_3D ( 'NONE', #5129, #1347, #6245 ) ;
#453 = EDGE_CURVE ( 'NONE', #421, #4626, #6250, .T. ) ;
#454 = DIRECTION ( 'NONE',  ( 0.1305261922200541547, -0.9914448613738101601, 0.000000000000000000 ) ) ;
#455 = CARTESIAN_POINT ( 'NONE',  ( -68.76644452187068168, 49.96174644486002592, 0.000000000000000000 ) ) ;
#456 = FILL_AREA_STYLE ('',( #4564 ) ) ;
#457 = DIRECTION ( 'NONE',  ( -0.000000000000000000, -0.000000000000000000, 1.000000000000000000 ) ) ;
#458 = CARTESIAN_POINT ( 'NONE',  ( -6.873268260756527152E-15, 0.000000000000000000, -79.99999999999995737 ) ) ;
#459 = ADVANCED_FACE ( 'NONE', ( #3218 ), #2157, .T. ) ;
#460 = ADVANCED_FACE ( 'NONE', ( #2627 ), #6369, .F. ) ;
#461 = ORIENTED_EDGE ( 'NONE', *, *, #895, .F. ) ;
#462 = AXIS2_PLACEMENT_3D ( 'NONE', #2816, #5271, #4796 ) ;
#463 = EDGE_CURVE ( 'NONE', #7599, #5285, #2102, .T. ) ;
#464 = ORIENTED_EDGE ( 'NONE', *, *, #7412, .F. ) ;
#465 = ORIENTED_EDGE ( 'NONE', *, *, #7115, .F. ) ;
#466 = CARTESIAN_POINT ( 'NONE',  ( 26.26644452187053957, 80.83980388508807380, 10.00000000000000000 ) ) ;
#467 = PLANE ( 'NONE',  #625 ) ;
#468 = AXIS2_PLACEMENT_3D ( 'NONE', #1319, #7361, #6181 ) ;
#469 = DIRECTION ( 'NONE',  ( 1.000000000000000000, 0.000000000000000000, 0.000000000000000000 ) ) ;
#470 = EDGE_CURVE ( 'NONE', #491, #1561, #4433, .T. ) ;
#471 = ADVANCED_FACE ( 'NONE', ( #4987 ), #1329, .T. ) ;
#472 = DIRECTION ( 'NONE',  ( 0.000000000000000000, 0.000000000000000000, 1.000000000000000000 ) ) ;
#473 = EDGE_LOOP ( 'NONE', ( #5151, #6491, #2990, #3433 ) ) ;
#474 = B_SPLINE_CURVE_WITH_KNOTS ( 'NONE', 3,
 ( #7048, #496, #2210, #412, #3419, #967, #6382, #2870 ),
 .UNSPECIFIED., .F., .F.,
 ( 4, 2, 2, 4 ),
 ( 0.004673709593152164388, 0.005837709341827651208, 0.007001709090503137160, 0.009329708587854108198 ),
 .UNSPECIFIED. ) ;
#475 = MANIFOLD_SOLID_BREP ( 'Body', #5362 ) ;
#476 = CIRCLE ( 'NONE', #4885, 6.099504629071904382 ) ;
#477 = LINE ( 'NONE', #2186, #2610 ) ;
#478 = DIRECTION ( 'NONE',  ( 1.000000000000000000, 0.000000000000000000, -0.000000000000000000 ) ) ;
#479 = CARTESIAN_POINT ( 'NONE',  ( -7.039801714450301422E-15, 0.000000000000000000, -82.99999999999995737 ) ) ;
#480 = AXIS2_PLACEMENT_3D ( 'NONE', #5844, #4103, #2188 ) ;
#481 = DIRECTION ( 'NONE',  ( -0.000000000000000000, -0.000000000000000000, -1.000000000000000000 ) ) ;
#482 = ORIENTED_EDGE ( 'NONE', *, *, #5916, .F. ) ;
#483 = EDGE_LOOP ( 'NONE', ( #1370, #2403, #2898 ) ) ;
#484 = AXIS2_PLACEMENT_3D ( 'NONE', #5502, #2370, #2407 ) ;
#485 = CARTESIAN_POINT ( 'NONE',  ( -6.689127551062010291, -5.375634714784629509, -0.3173508448886595557 ) ) ;
#486 = CARTESIAN_POINT ( 'NONE',  ( -350.0000000000000000, 300.0000000000001137, -120.0000000000000000 ) ) ;
#487 = CARTESIAN_POINT ( 'NONE',  ( 0.000000000000000000, 1.484218055610305731, -3.000000000000000000 ) ) ;
#488 = DIRECTION ( 'NONE',  ( -1.000000000000000000, 0.000000000000000000, 0.000000000000000000 ) ) ;
#489 = AXIS2_PLACEMENT_3D ( 'NONE', #1675, #1035, #3446 ) ;
#490 = DIRECTION ( 'NONE',  ( 0.000000000000000000, 0.000000000000000000, -1.000000000000000000 ) ) ;
#491 = VERTEX_POINT ( 'NONE', #486 ) ;
#492 = ORIENTED_EDGE ( 'NONE', *, *, #2605, .F. ) ;
#493 = ORIENTED_EDGE ( 'NONE', *, *, #81, .F. ) ;
#494 = AXIS2_PLACEMENT_3D ( 'NONE', #1361, #3659, #3110 ) ;
#495 = CARTESIAN_POINT ( 'NONE',  ( 0.000000000000000000, 0.000000000000000000, 0.000000000000000000 ) ) ;
#496 = CARTESIAN_POINT ( 'NONE',  ( 4.339467034331189410, 6.732211846623394003, 4.972295158619556565E-15 ) ) ;
#497 = CARTESIAN_POINT ( 'NONE',  ( 31.51644452187053602, 80.83980388508807380, 10.00000000000000000 ) ) ;
#498 = DIRECTION ( 'NONE',  ( 0.000000000000000000, 0.000000000000000000, 1.000000000000000000 ) ) ;
#499 = DIRECTION ( 'NONE',  ( 1.000000000000000000, 0.000000000000000000, 0.000000000000000000 ) ) ;
#500 = CYLINDRICAL_SURFACE ( 'NONE', #990, 28.49999999999999645 ) ;
#501 = CIRCLE ( 'NONE', #6302, 279.9963296805736945 ) ;
#502 = VERTEX_POINT ( 'NONE', #3884 ) ;
#503 = ORIENTED_EDGE ( 'NONE', *, *, #3907, .F. ) ;
#504 = ORIENTED_EDGE ( 'NONE', *, *, #2684, .F. ) ;
#505 = LINE ( 'NONE', #547, #511 ) ;
#506 = FACE_OUTER_BOUND ( 'NONE', #4471, .T. ) ;
#507 = SURFACE_STYLE_FILL_AREA ( #427 ) ;
#508 = EDGE_CURVE ( 'NONE', #57, #5308, #1029, .T. ) ;
#509 = CARTESIAN_POINT ( 'NONE',  ( -68.76644452187072432, 49.96174644486006855, -134.1720000000000255 ) ) ;
#510 = ORIENTED_EDGE ( 'NONE', *, *, #6970, .F. ) ;
#511 = VECTOR ( 'NONE', #2920, 999.9999999999998863 ) ;
#512 = EDGE_CURVE ( 'NONE', #3634, #5216, #2318, .T. ) ;
#513 = FACE_OUTER_BOUND ( 'NONE', #3270, .T. ) ;
#514 = CARTESIAN_POINT ( 'NONE',  ( 0.000000000000000000, 0.000000000000000000, -4.700000000000000178 ) ) ;
#515 = AXIS2_PLACEMENT_3D ( 'NONE', #5037, #3898, #818 ) ;
#516 =( REPRESENTATION_RELATIONSHIP ('NONE','NONE', #1229, #1433 ) REPRESENTATION_RELATIONSHIP_WITH_TRANSFORMATION ( #445 )SHAPE_REPRESENTATION_RELATIONSHIP( ) );
#517 = CARTESIAN_POINT ( 'NONE',  ( 0.000000000000000000, 0.000000000000000000, -3.000000000000000000 ) ) ;
#518 = CARTESIAN_POINT ( 'NONE',  ( 29.99999999999999289, 0.000000000000000000, -139.9999999999999716 ) ) ;
#519 = ORIENTED_EDGE ( 'NONE', *, *, #5812, .T. ) ;
#520 = VERTEX_POINT ( 'NONE', #2940 ) ;
#521 = ADVANCED_FACE ( 'NONE', ( #3486 ), #1713, .F. ) ;
#522 = CARTESIAN_POINT ( 'NONE',  ( 39.64284999284934941, 144.6666666666667140, 5.000000000000000000 ) ) ;
#523 = LINE ( 'NONE', #6483, #1208 ) ;
#524 = CARTESIAN_POINT ( 'NONE',  ( -1.852913429038039572, -299.9999999999999432, -120.0000000000000000 ) ) ;
#525 = MANIFOLD_SOLID_BREP ( 'M10 Clearance Hole1', #6120 ) ;
#526 = FACE_OUTER_BOUND ( 'NONE', #5662, .T. ) ;
#527 = CARTESIAN_POINT ( 'NONE',  ( 28.49999999999999645, 0.000000000000000000, -3.000000000000000000 ) ) ;
#528 = CYLINDRICAL_SURFACE ( 'NONE', #6274, 1.250000000000000222 ) ;
#529 = EDGE_CURVE ( 'NONE', #6340, #6348, #6500, .T. ) ;
#530 = CONTEXT_DEPENDENT_SHAPE_REPRESENTATION ( #914, #1966 ) ;
#531 = VECTOR ( 'NONE', #6993, 1000.000000000000114 ) ;
#532 = DIRECTION ( 'NONE',  ( -0.000000000000000000, -0.000000000000000000, 1.000000000000000000 ) ) ;
#533 = ORIENTED_EDGE ( 'NONE', *, *, #7554, .T. ) ;
#534 = ORIENTED_EDGE ( 'NONE', *, *, #2929, .F. ) ;
#535 = CIRCLE ( 'NONE', #660, 4.999999999999990230 ) ;
#536 = CARTESIAN_POINT ( 'NONE',  ( -6.686525924292792133, 5.377136764700155780, -0.3167204509598384177 ) ) ;
#537 = CARTESIAN_POINT ( 'NONE',  ( 8.000000000000000000, -3.098204225878171680, -0.3157906771918751465 ) ) ;
#538 = CYLINDRICAL_SURFACE ( 'NONE', #6515, 28.50000000000000711 ) ;
#539 = DIRECTION ( 'NONE',  ( 0.000000000000000000, 0.000000000000000000, -1.000000000000000000 ) ) ;
#540 = SURFACE_STYLE_FILL_AREA ( #4644 ) ;
#541 = DIRECTION ( 'NONE',  ( 1.000000000000000000, 0.000000000000000000, 0.000000000000000000 ) ) ;
#542 = AXIS2_PLACEMENT_3D ( 'NONE', #7456, #6279, #2065 ) ;
#543 = EDGE_LOOP ( 'NONE', ( #5445, #2673, #6980, #2672 ) ) ;
#544 = VERTEX_POINT ( 'NONE', #2194 ) ;
#545 = VERTEX_POINT ( 'NONE', #7662 ) ;
#546 = AXIS2_PLACEMENT_3D ( 'NONE', #386, #1018, #2806 ) ;
#547 = CARTESIAN_POINT ( 'NONE',  ( 5.459126460941067016, -34.89491303563345070, -3.000000000000000000 ) ) ;
#548 = CARTESIAN_POINT ( 'NONE',  ( 350.0000000000000000, 37.15382499588017140, -1041.954445729288636 ) ) ;
#549 = DIRECTION ( 'NONE',  ( 1.000000000000000000, 0.000000000000000000, 0.000000000000000000 ) ) ;
#550 = AXIS2_PLACEMENT_3D ( 'NONE', #3748, #3669, #5598 ) ;
#551 = ORIENTED_EDGE ( 'NONE', *, *, #3232, .F. ) ;
#552 = AXIS2_PLACEMENT_3D ( 'NONE', #3996, #7623, #7504 ) ;
#553 = EDGE_LOOP ( 'NONE', ( #2394, #4192, #566, #4577 ) ) ;
#554 = CYLINDRICAL_SURFACE ( 'NONE', #7508, 150.0000000000000568 ) ;
#555 = DIRECTION ( 'NONE',  ( -0.000000000000000000, -0.000000000000000000, 1.000000000000000000 ) ) ;
#556 = MECHANICAL_DESIGN_GEOMETRIC_PRESENTATION_REPRESENTATION (  '', ( #1054 ), #799 ) ;
#557 = AXIS2_PLACEMENT_3D ( 'NONE', #5104, #4513, #3373 ) ;
#558 = EDGE_CURVE ( 'NONE', #1483, #3701, #583, .T. ) ;
#559 = CARTESIAN_POINT ( 'NONE',  ( -10.00000000000000000, 28.28427124746189136, 10.00000000000000000 ) ) ;
#560 = EDGE_CURVE ( 'NONE', #7291, #3873, #1586, .T. ) ;
#561 = ORIENTED_EDGE ( 'NONE', *, *, #5713, .F. ) ;
#562 = EDGE_CURVE ( 'NONE', #1095, #2283, #523, .T. ) ;
#563 = ORIENTED_EDGE ( 'NONE', *, *, #6161, .F. ) ;
#564 = VECTOR ( 'NONE', #809, 1000.000000000000000 ) ;
#565 = EDGE_CURVE ( 'NONE', #2154, #3857, #3355, .T. ) ;
#566 = ORIENTED_EDGE ( 'NONE', *, *, #3757, .F. ) ;
#567 = APPLICATION_CONTEXT ( 'automotive_design' ) ;
#568 = CARTESIAN_POINT ( 'NONE',  ( -1.677050983124841466, 3.949485927250214050E-15, 32.25000000000000000 ) ) ;
#569 = DIRECTION ( 'NONE',  ( 1.000000000000000000, -1.586032892321652729E-16, 0.000000000000000000 ) ) ;
#570 = DIRECTION ( 'NONE',  ( 0.000000000000000000, 0.000000000000000000, 1.000000000000000000 ) ) ;
#571 = DIRECTION ( 'NONE',  ( 0.000000000000000000, 0.000000000000000000, -1.000000000000000000 ) ) ;
#572 = ITEM_DEFINED_TRANSFORMATION ( 'NONE', 'NONE', #7253,  #7485 ) ;
#573 = EDGE_CURVE ( 'NONE', #6864, #6819, #3734, .T. ) ;
#574 =( GEOMETRIC_REPRESENTATION_CONTEXT ( 3 ) GLOBAL_UNCERTAINTY_ASSIGNED_CONTEXT ( ( #5327 ) ) GLOBAL_UNIT_ASSIGNED_CONTEXT ( ( #4488, #1529, #2096 ) ) REPRESENTATION_CONTEXT ( 'NONE', 'WORKASPACE' ) );
#575 = DIRECTION ( 'NONE',  ( 1.000000000000000000, 0.000000000000000000, 0.000000000000000000 ) ) ;
#576 = CIRCLE ( 'NONE', #3727, 1.250000000000000222 ) ;
#577 = EDGE_LOOP ( 'NONE', ( #2999, #4050 ) ) ;
#578 = VERTEX_POINT ( 'NONE', #6013 ) ;
#579 = CARTESIAN_POINT ( 'NONE',  ( -68.76644452187068168, 49.96174644486002592, 0.000000000000000000 ) ) ;
#580 = CARTESIAN_POINT ( 'NONE',  ( 10.00000000000000000, 28.28427124746190202, 0.000000000000000000 ) ) ;
#581 = PLANE ( 'NONE',  #2500 ) ;
#582 = DIRECTION ( 'NONE',  ( -3.081487911019577365E-33, 2.775557561562891967E-17, 1.000000000000000000 ) ) ;
#583 = CIRCLE ( 'NONE', #702, 29.99999999999999289 ) ;
#584 = SURFACE_STYLE_USAGE ( .BOTH. , #4799 ) ;
#585 = CARTESIAN_POINT ( 'NONE',  ( 4.681481898397002794, -6.534749472788152325, -3.252606517456513302E-16 ) ) ;
#586 = ORIENTED_EDGE ( 'NONE', *, *, #1973, .F. ) ;
#587 = VERTEX_POINT ( 'NONE', #644 ) ;
#588 = CIRCLE ( 'NONE', #4736, 5.249999999999991118 ) ;
#589 = VERTEX_POINT ( 'NONE', #4784 ) ;
#590 = DIRECTION ( 'NONE',  ( 0.000000000000000000, -0.000000000000000000, -1.000000000000000000 ) ) ;
#591 = CARTESIAN_POINT ( 'NONE',  ( -8.000000000000000000, -4.618802153517013842, -0.7145311798163319628 ) ) ;
#592 = CARTESIAN_POINT ( 'NONE',  ( -279.9963296805736945, 3.428966089163216048E-14, -82.99999999999998579 ) ) ;
#593 = B_SPLINE_CURVE_WITH_KNOTS ( 'NONE', 3,
 ( #6364, #1707, #3521, #3990, #4698, #6519, #3366, #987 ),
 .UNSPECIFIED., .F., .F.,
 ( 4, 2, 2, 4 ),
 ( 0.004673709593152171327, 0.005837709341827658147, 0.007001709090503144099, 0.009329708587854113402 ),
 .UNSPECIFIED. ) ;
#594 = ORIENTED_EDGE ( 'NONE', *, *, #7692, .T. ) ;
#595 = ORIENTED_EDGE ( 'NONE', *, *, #2057, .F. ) ;
#596 = CARTESIAN_POINT ( 'NONE',  ( 0.000000000000000000, 0.000000000000000000, -79.99999999999995737 ) ) ;
#597 = CYLINDRICAL_SURFACE ( 'NONE', #4258, 29.99999999999999289 ) ;
#598 = DIRECTION ( 'NONE',  ( 1.000000000000000000, 0.000000000000000000, 0.000000000000000000 ) ) ;
#599 = VERTEX_POINT ( 'NONE', #3056 ) ;
#600 = VECTOR ( 'NONE', #7039, 1000.000000000000000 ) ;
#601 = EDGE_CURVE ( 'NONE', #3231, #6794, #5455, .T. ) ;
#602 = ORIENTED_EDGE ( 'NONE', *, *, #3937, .F. ) ;
#603 = DIRECTION ( 'NONE',  ( 0.000000000000000000, 0.000000000000000000, 1.000000000000000000 ) ) ;
#604 = DIRECTION ( 'NONE',  ( -0.000000000000000000, -0.000000000000000000, -1.000000000000000000 ) ) ;
#605 = ADVANCED_FACE ( 'NONE', ( #1152 ), #4305, .T. ) ;
#606 = CIRCLE ( 'NONE', #5134, 7.999999999999998224 ) ;
#607 = CARTESIAN_POINT ( 'NONE',  ( 0.000000000000000000, 0.000000000000000000, -50.00000000000000000 ) ) ;
#608 = PLANE ( 'NONE',  #1351 ) ;
#609 = CONTEXT_DEPENDENT_SHAPE_REPRESENTATION ( #7272, #4847 ) ;
#610 = EDGE_CURVE ( 'NONE', #7629, #6982, #1196, .T. ) ;
#611 = CARTESIAN_POINT ( 'NONE',  ( -2.750000000000000000, -33.63777638310832430, 0.000000000000000000 ) ) ;
#612 = AXIS2_PLACEMENT_3D ( 'NONE', #3104, #6064, #4946 ) ;
#613 = ORIENTED_EDGE ( 'NONE', *, *, #2264, .T. ) ;
#614 = VECTOR ( 'NONE', #286, 1000.000000000000000 ) ;
#615 = CARTESIAN_POINT ( 'NONE',  ( -9.702951051037022268, -29.86427928513813512, -3.000000000000000000 ) ) ;
#616 = EDGE_CURVE ( 'NONE', #7044, #7003, #5625, .T. ) ;
#617 = AXIS2_PLACEMENT_3D ( 'NONE', #4825, #53, #3645 ) ;
#618 = FACE_OUTER_BOUND ( 'NONE', #3198, .T. ) ;
#619 = CARTESIAN_POINT ( 'NONE',  ( 0.3344772040064616925, 0.000000000000000000, 0.000000000000000000 ) ) ;
#620 = CARTESIAN_POINT ( 'NONE',  ( -119.9981648402875436, 207.8429183184017575, -124.7000000000000028 ) ) ;
#621 = DIRECTION ( 'NONE',  ( 1.000000000000000000, -1.586032892321652729E-16, 0.000000000000000000 ) ) ;
#622 = DIRECTION ( 'NONE',  ( 1.000000000000000000, 0.000000000000000000, 0.000000000000000000 ) ) ;
#623 = DIRECTION ( 'NONE',  ( -0.9997999799959990108, -0.01999999999999999001, 0.000000000000000000 ) ) ;
#624 = ORIENTED_EDGE ( 'NONE', *, *, #2405, .T. ) ;
#625 = AXIS2_PLACEMENT_3D ( 'NONE', #5366, #6465, #5319 ) ;
#626 = ORIENTED_EDGE ( 'NONE', *, *, #707, .F. ) ;
#627 =( REPRESENTATION_RELATIONSHIP ('NONE','NONE', #1229, #2051 ) REPRESENTATION_RELATIONSHIP_WITH_TRANSFORMATION ( #6373 )SHAPE_REPRESENTATION_RELATIONSHIP( ) );
#628 = ORIENTED_EDGE ( 'NONE', *, *, #2216, .T. ) ;
#629 = CARTESIAN_POINT ( 'NONE',  ( -1.728922298134113098E-15, 8.513302795252935035E-16, 10.00000000000000000 ) ) ;
#630 =( GEOMETRIC_REPRESENTATION_CONTEXT ( 3 ) GLOBAL_UNCERTAINTY_ASSIGNED_CONTEXT ( ( #1956 ) ) GLOBAL_UNIT_ASSIGNED_CONTEXT ( ( #5597, #5554, #3667 ) ) REPRESENTATION_CONTEXT ( 'NONE', 'WORKASPACE' ) );
#631 = CARTESIAN_POINT ( 'NONE',  ( 0.000000000000000000, -150.0000000000000568, 10.00000000000000000 ) ) ;
#632 = EDGE_CURVE ( 'NONE', #7413, #257, #5381, .T. ) ;
#633 = PRODUCT_DEFINITION_SHAPE ( 'NONE', 'NONE',  #7784 ) ;
#634 = ORIENTED_EDGE ( 'NONE', *, *, #7223, .T. ) ;
#635 = ORIENTED_EDGE ( 'NONE', *, *, #878, .T. ) ;
#636 = AXIS2_PLACEMENT_3D ( 'NONE', #596, #7064, #5883 ) ;
#637 = SHAPE_REPRESENTATION ( 'Pocketed Starwheel', ( #7485 ), #2086 ) ;
#638 = CARTESIAN_POINT ( 'NONE',  ( -199.9963296805737230, 2.449248649845333917E-14, -82.99999999999998579 ) ) ;
#639 = FACE_OUTER_BOUND ( 'NONE', #3468, .T. ) ;
#640 = CIRCLE ( 'NONE', #5305, 7.999999999999998224 ) ;
#641 = DIRECTION ( 'NONE',  ( 0.000000000000000000, 0.000000000000000000, 1.000000000000000000 ) ) ;
#642 = EDGE_LOOP ( 'NONE', ( #3769, #1334 ) ) ;
#643 = ORIENTED_EDGE ( 'NONE', *, *, #5237, .F. ) ;
#644 = CARTESIAN_POINT ( 'NONE',  ( 29.99999999999999289, 0.000000000000000000, -60.00000000000000000 ) ) ;
#645 = CARTESIAN_POINT ( 'NONE',  ( -5.459126460941067016, -34.89491303563345070, -3.000000000000000000 ) ) ;
#646 = DIRECTION ( 'NONE',  ( -0.000000000000000000, -0.000000000000000000, -1.000000000000000000 ) ) ;
#647 = LINE ( 'NONE', #93, #4504 ) ;
#648 = DIRECTION ( 'NONE',  ( 0.000000000000000000, 0.000000000000000000, 1.000000000000000000 ) ) ;
#649 = PRODUCT_RELATED_PRODUCT_CATEGORY ( 'part', '', ( #3788 ) ) ;
#650 = ORIENTED_EDGE ( 'NONE', *, *, #4418, .F. ) ;
#651 = DIRECTION ( 'NONE',  ( -0.000000000000000000, -0.000000000000000000, 1.000000000000000000 ) ) ;
#652 = FACE_BOUND ( 'NONE', #7710, .T. ) ;
#653 = CARTESIAN_POINT ( 'NONE',  ( -39.64284999284935651, 144.6666666666667140, 10.00000000000000000 ) ) ;
#654 = CARTESIAN_POINT ( 'NONE',  ( 122.8429183184020985, 119.9981648402858383, 0.000000000000000000 ) ) ;
#655 = SURFACE_STYLE_FILL_AREA ( #6777 ) ;
#656 = LINE ( 'NONE', #1850, #7180 ) ;
#657 = CARTESIAN_POINT ( 'NONE',  ( 37.49999999999997868, 4.592425496802572000E-15, -112.9999999999999716 ) ) ;
#658 = ADVANCED_FACE ( 'NONE', ( #4193 ), #3609, .F. ) ;
#659 = ORIENTED_EDGE ( 'NONE', *, *, #7204, .T. ) ;
#660 = AXIS2_PLACEMENT_3D ( 'NONE', #1803, #3650, #4750 ) ;
#661 = ORIENTED_EDGE ( 'NONE', *, *, #6270, .T. ) ;
#662 = EDGE_CURVE ( 'NONE', #1120, #6644, #7383, .T. ) ;
#663 = ORIENTED_EDGE ( 'NONE', *, *, #7369, .T. ) ;
#664 = DIRECTION ( 'NONE',  ( 1.000000000000000000, 0.000000000000000000, 0.000000000000000000 ) ) ;
#665 = AXIS2_PLACEMENT_3D ( 'NONE', #4618, #472, #430 ) ;
#666 = AXIS2_PLACEMENT_3D ( 'NONE', #3224, #6851, #4477 ) ;
#667 = LINE ( 'NONE', #5442, #3443 ) ;
#668 = EDGE_CURVE ( 'NONE', #3544, #1948, #6635, .T. ) ;
#669 = VERTEX_POINT ( 'NONE', #3097 ) ;
#670 = EDGE_LOOP ( 'NONE', ( #4030, #5229, #7475 ) ) ;
#671 = VECTOR ( 'NONE', #569, 1000.000000000000000 ) ;
#672 = EDGE_CURVE ( 'NONE', #3192, #3615, #90, .T. ) ;
#673 = DIRECTION ( 'NONE',  ( -1.000000000000000000, 0.000000000000000000, 0.000000000000000000 ) ) ;
#674 = DIRECTION ( 'NONE',  ( 0.1305261922200541547, -0.9914448613738101601, 0.000000000000000000 ) ) ;
#675 = CARTESIAN_POINT ( 'NONE',  ( -279.9963296805736945, 3.428966089163216048E-14, 10.00000000000000000 ) ) ;
#676 = CONICAL_SURFACE ( 'NONE', #6724, 4.999999999999990230, 0.7853981633974524978 ) ;
#677 = DIRECTION ( 'NONE',  ( -0.000000000000000000, -0.000000000000000000, 1.000000000000000000 ) ) ;
#678 = ORIENTED_EDGE ( 'NONE', *, *, #6796, .T. ) ;
#679 = ORIENTED_EDGE ( 'NONE', *, *, #312, .F. ) ;
#680 = PRESENTATION_LAYER_ASSIGNMENT (  '', '', ( #3832 ) ) ;
#681 = VECTOR ( 'NONE', #5176, 1000.000000000000000 ) ;
#682 = CARTESIAN_POINT ( 'NONE',  ( 3.716043017018883621, 28.25669875083898930, 13.00000000000000178 ) ) ;
#683 = CARTESIAN_POINT ( 'NONE',  ( -26.82422866010495710, -9.628642520646591763, -122.9999999999999716 ) ) ;
#684 = DIRECTION ( 'NONE',  ( -0.000000000000000000, 0.000000000000000000, -1.000000000000000000 ) ) ;
#685 = DIRECTION ( 'NONE',  ( 0.000000000000000000, 0.000000000000000000, 1.000000000000000000 ) ) ;
#686 = CONTEXT_DEPENDENT_SHAPE_REPRESENTATION ( #6572, #1898 ) ;
#687 = DIRECTION ( 'NONE',  ( -0.000000000000000000, -0.000000000000000000, 1.000000000000000000 ) ) ;
#688 = VERTEX_POINT ( 'NONE', #568 ) ;
#689 = PRESENTATION_LAYER_ASSIGNMENT (  '', '', ( #5219 ) ) ;
#690 = DIRECTION ( 'NONE',  ( 1.000000000000000000, 0.000000000000000000, 0.000000000000000000 ) ) ;
#691 = CARTESIAN_POINT ( 'NONE',  ( -8.000000000000000000, 9.797174393178825657E-16, 2.573333333333333695 ) ) ;
#692 = DIRECTION ( 'NONE',  ( 0.000000000000000000, 0.000000000000000000, 1.000000000000000000 ) ) ;
#693 = DIRECTION ( 'NONE',  ( -7.231745315385741915E-18, 4.951172373687671349E-17, -0.9999999999999998890 ) ) ;
#694 = PRODUCT_DEFINITION_SHAPE ( 'NONE', 'NONE',  #7785 ) ;
#695 = CARTESIAN_POINT ( 'NONE',  ( -4.250000000000000000, 5.204748896376250699E-16, -4.700000000000000178 ) ) ;
#696 = CARTESIAN_POINT ( 'NONE',  ( -73.76644452187066747, 49.96174644486002592, 24.17200000000001125 ) ) ;
#697 = CARTESIAN_POINT ( 'NONE',  ( -68.76644452187068168, 49.96174644486002592, -40.00000000000000000 ) ) ;
#698 = ORIENTED_EDGE ( 'NONE', *, *, #2750, .F. ) ;
#699 = VERTEX_POINT ( 'NONE', #1951 ) ;
#700 = ADVANCED_FACE ( 'NONE', ( #3679 ), #2979, .T. ) ;
#701 = ORIENTED_EDGE ( 'NONE', *, *, #2330, .F. ) ;
#702 = AXIS2_PLACEMENT_3D ( 'NONE', #2238, #7036, #2274 ) ;
#703 = CARTESIAN_POINT ( 'NONE',  ( 37.49999999999997868, 4.592425496802572000E-15, -119.9999999999999858 ) ) ;
#704 = ADVANCED_FACE ( 'NONE', ( #6716 ), #7273, .F. ) ;
#705 = EDGE_CURVE ( 'NONE', #219, #1120, #6679, .T. ) ;
#706 = DIRECTION ( 'NONE',  ( -0.000000000000000000, 1.000000000000000000, 0.000000000000000000 ) ) ;
#707 = EDGE_CURVE ( 'NONE', #2049, #6833, #1270, .T. ) ;
#708 = ORIENTED_EDGE ( 'NONE', *, *, #3264, .T. ) ;
#709 = CIRCLE ( 'NONE', #6257, 28.50000000000000711 ) ;
#710 = ORIENTED_EDGE ( 'NONE', *, *, #4511, .F. ) ;
#711 = CYLINDRICAL_SURFACE ( 'NONE', #6817, 29.99999999999999289 ) ;
#712 = ADVANCED_FACE ( 'NONE', ( #6130 ), #4936, .T. ) ;
#713 = CARTESIAN_POINT ( 'NONE',  ( 8.000000000000000000, 3.115336682267008328, -0.3193931313915058801 ) ) ;
#714 = AXIS2_PLACEMENT_3D ( 'NONE', #3882, #3330, #2041 ) ;
#715 = FACE_OUTER_BOUND ( 'NONE', #6738, .T. ) ;
#716 = CARTESIAN_POINT ( 'NONE',  ( 8.000000000000001776, -1.555946510856142551, -4.632911297836646014 ) ) ;
#717 = ORIENTED_EDGE ( 'NONE', *, *, #5240, .F. ) ;
#718 = CIRCLE ( 'NONE', #468, 5.250000000000004441 ) ;
#719 = VERTEX_POINT ( 'NONE', #2731 ) ;
#720 = DIRECTION ( 'NONE',  ( 0.000000000000000000, 0.000000000000000000, -1.000000000000000000 ) ) ;
#721 = CARTESIAN_POINT ( 'NONE',  ( 89.90381056766497636, 75.00000000000153477, 0.000000000000000000 ) ) ;
#722 = LINE ( 'NONE', #6945, #1174 ) ;
#723 = CARTESIAN_POINT ( 'NONE',  ( 6.713333333332999864, 0.000000000000000000, 2.573333333332999739 ) ) ;
#724 = VECTOR ( 'NONE', #4787, 1000.000000000000000 ) ;
#725 = CARTESIAN_POINT ( 'NONE',  ( -8.000000000000000000, 4.618802153517013842, -3.985468820183668104 ) ) ;
#726 = ORIENTED_EDGE ( 'NONE', *, *, #6984, .F. ) ;
#727 = VECTOR ( 'NONE', #7229, 1000.000000000000000 ) ;
#728 = FACE_BOUND ( 'NONE', #6470, .T. ) ;
#729 = CARTESIAN_POINT ( 'NONE',  ( -3.499999999999996447, 35.97500000000000142, 0.000000000000000000 ) ) ;
#730 = CYLINDRICAL_SURFACE ( 'NONE', #6902, 5.249999999999983125 ) ;
#731 = APPLICATION_PROTOCOL_DEFINITION ( 'draft international standard', 'automotive_design', 1998, #2446 ) ;
#732 = CARTESIAN_POINT ( 'NONE',  ( -63.76644452187073142, 49.96174644486006855, -134.1720000000000255 ) ) ;
#733 = CARTESIAN_POINT ( 'NONE',  ( 0.5700000000000001732, -28.49429942988597020, -3.000000000000000000 ) ) ;
#734 = CARTESIAN_POINT ( 'NONE',  ( -114.7481648402875578, 207.8429183184017859, -50.00000000000000000 ) ) ;
#735 = ORIENTED_EDGE ( 'NONE', *, *, #1621, .F. ) ;
#736 = VERTEX_POINT ( 'NONE', #2149 ) ;
#737 = AXIS2_PLACEMENT_3D ( 'NONE', #7008, #6455, #5943 ) ;
#738 = VERTEX_POINT ( 'NONE', #5093 ) ;
#739 = DIRECTION ( 'NONE',  ( -0.000000000000000000, -0.000000000000000000, -1.000000000000000000 ) ) ;
#740 = LINE ( 'NONE', #1932, #373 ) ;
#741 =( NAMED_UNIT ( * ) SI_UNIT ( $, .STERADIAN. ) SOLID_ANGLE_UNIT ( ) );
#742 = LINE ( 'NONE', #6704, #5973 ) ;
#743 = VECTOR ( 'NONE', #6568, 1000.000000000000114 ) ;
#744 = ORIENTED_EDGE ( 'NONE', *, *, #4992, .F. ) ;
#745 = ORIENTED_EDGE ( 'NONE', *, *, #3810, .T. ) ;
#746 = VERTEX_POINT ( 'NONE', #907 ) ;
#747 = ADVANCED_FACE ( 'NONE', ( #5569 ), #317, .T. ) ;
#748 = CARTESIAN_POINT ( 'NONE',  ( -64.59444452187072727, 49.96174644486006855, -135.0000000000000000 ) ) ;
#749 = FILL_AREA_STYLE ('',( #5523 ) ) ;
#750 = DIRECTION ( 'NONE',  ( 0.000000000000000000, 0.000000000000000000, 1.000000000000000000 ) ) ;
#751 = FACE_OUTER_BOUND ( 'NONE', #3367, .T. ) ;
#752 = ORIENTED_EDGE ( 'NONE', *, *, #2539, .T. ) ;
#753 = VECTOR ( 'NONE', #260, 1000.000000000000000 ) ;
#754 = EDGE_CURVE ( 'NONE', #7338, #2067, #1723, .T. ) ;
#755 = EDGE_LOOP ( 'NONE', ( #5490, #6461, #7212, #2166 ) ) ;
#756 = PRODUCT_DEFINITION_SHAPE ( 'NONE', 'NONE',  #7799 ) ;
#757 = EDGE_CURVE ( 'NONE', #3192, #1710, #4102, .T. ) ;
#758 = CARTESIAN_POINT ( 'NONE',  ( 0.000000000000000000, 0.000000000000000000, -50.00000000000004263 ) ) ;
#759 = DIRECTION ( 'NONE',  ( 0.000000000000000000, 0.000000000000000000, -1.000000000000000000 ) ) ;
#760 = CIRCLE ( 'NONE', #7682, 40.00000000000001421 ) ;
#761 = DIRECTION ( 'NONE',  ( 0.000000000000000000, 0.000000000000000000, 1.000000000000000000 ) ) ;
#762 = DIRECTION ( 'NONE',  ( -0.000000000000000000, -0.000000000000000000, -1.000000000000000000 ) ) ;
#763 = EDGE_LOOP ( 'NONE', ( #3582, #5792, #5209, #744 ) ) ;
#764 = ADVANCED_FACE ( 'NONE', ( #6171 ), #6323, .F. ) ;
#765 = AXIS2_PLACEMENT_3D ( 'NONE', #3393, #1015, #7018 ) ;
#766 = FACE_OUTER_BOUND ( 'NONE', #2228, .T. ) ;
#767 = FACE_OUTER_BOUND ( 'NONE', #7254, .T. ) ;
#768 = EDGE_CURVE ( 'NONE', #3595, #3008, #6005, .T. ) ;
#769 = DIRECTION ( 'NONE',  ( 0.000000000000000000, 1.000000000000000000, -1.224646799147353207E-16 ) ) ;
#770 = DIRECTION ( 'NONE',  ( -0.1555099737793451398, 0.9878343221690302212, -1.110223024625155986E-18 ) ) ;
#771 = SHAPE_DEFINITION_REPRESENTATION ( #1259, #2051 ) ;
#772 = CARTESIAN_POINT ( 'NONE',  ( 0.000000000000000000, 0.000000000000000000, 3.859999999999999876 ) ) ;
#773 = EDGE_LOOP ( 'NONE', ( #447, #3094 ) ) ;
#774 = EDGE_LOOP ( 'NONE', ( #3751, #5530 ) ) ;
#775 = EDGE_LOOP ( 'NONE', ( #5683, #7161, #971, #2534, #5294, #5753, #1571, #266 ) ) ;
#776 = LINE ( 'NONE', #1405, #2918 ) ;
#777 = CARTESIAN_POINT ( 'NONE',  ( 4.681481898397003683, -6.534749472788152325, -4.700000000000000178 ) ) ;
#778 = CARTESIAN_POINT ( 'NONE',  ( -7.039801714450301422E-15, 0.000000000000000000, -82.99999999999995737 ) ) ;
#779 = AXIS2_PLACEMENT_3D ( 'NONE', #837, #6286, #2075 ) ;
#780 = ORIENTED_EDGE ( 'NONE', *, *, #6297, .F. ) ;
#781 = ORIENTED_EDGE ( 'NONE', *, *, #6160, .T. ) ;
#782 = AXIS2_PLACEMENT_3D ( 'NONE', #13, #2471, #1266 ) ;
#783 = PRODUCT_DEFINITION_FORMATION_WITH_SPECIFIED_SOURCE ( 'ANY', '', #131, .NOT_KNOWN. ) ;
#784 = CARTESIAN_POINT ( 'NONE',  ( -74.01644452187068168, 49.96174644486002592, 0.000000000000000000 ) ) ;
#785 = DIRECTION ( 'NONE',  ( -0.000000000000000000, -0.000000000000000000, 1.000000000000000000 ) ) ;
#786 = CARTESIAN_POINT ( 'NONE',  ( 2.309976723937608778, -7.903938623646878270, -0.1306530452038152101 ) ) ;
#787 = CIRCLE ( 'NONE', #5332, 5.000000000000000888 ) ;
#788 = ORIENTED_EDGE ( 'NONE', *, *, #5777, .T. ) ;
#789 = EDGE_CURVE ( 'NONE', #4399, #185, #6381, .T. ) ;
#790 = CARTESIAN_POINT ( 'NONE',  ( -2.309976723937612331, 7.903938623646864059, -0.1306530452038102419 ) ) ;
#791 = CARTESIAN_POINT ( 'NONE',  ( -3.499999999999996003, 0.000000000000000000, 0.000000000000000000 ) ) ;
#792 = VECTOR ( 'NONE', #1139, 1000.000000000000000 ) ;
#793 = CARTESIAN_POINT ( 'NONE',  ( 0.000000000000000000, 1.484218055610305731, 0.000000000000000000 ) ) ;
#794 = EDGE_CURVE ( 'NONE', #502, #2536, #6762, .T. ) ;
#795 = EDGE_CURVE ( 'NONE', #3391, #5308, #239, .T. ) ;
#796 = DIRECTION ( 'NONE',  ( -0.000000000000000000, -0.000000000000000000, 1.000000000000000000 ) ) ;
#797 = ORIENTED_EDGE ( 'NONE', *, *, #4469, .F. ) ;
#798 = ADVANCED_FACE ( 'NONE', ( #4978 ), #2695, .T. ) ;
#799 =( GEOMETRIC_REPRESENTATION_CONTEXT ( 3 ) GLOBAL_UNCERTAINTY_ASSIGNED_CONTEXT ( ( #6208 ) ) GLOBAL_UNIT_ASSIGNED_CONTEXT ( ( #6695, #3035, #7249 ) ) REPRESENTATION_CONTEXT ( 'NONE', 'WORKASPACE' ) );
#800 = CIRCLE ( 'NONE', #1055, 5.249999999999976907 ) ;
#801 = DIRECTION ( 'NONE',  ( -0.000000000000000000, -0.000000000000000000, -1.000000000000000000 ) ) ;
#802 = CARTESIAN_POINT ( 'NONE',  ( -6.713333333332999864, 8.221462178275489009E-16, 2.573333333332999739 ) ) ;
#803 = EDGE_CURVE ( 'NONE', #1238, #1502, #588, .T. ) ;
#804 = FACE_OUTER_BOUND ( 'NONE', #126, .T. ) ;
#805 = DIRECTION ( 'NONE',  ( 0.000000000000000000, 0.000000000000000000, 1.000000000000000000 ) ) ;
#806 = APPLICATION_PROTOCOL_DEFINITION ( 'draft international standard', 'automotive_design', 1998, #3243 ) ;
#807 = CIRCLE ( 'NONE', #7607, 31.52499999999999858 ) ;
#808 = COLOUR_RGB ( '',0.8941176470588234615, 0.8941176470588234615, 0.8941176470588234615 ) ;
#809 = DIRECTION ( 'NONE',  ( 1.000000000000000000, 0.000000000000000000, 0.000000000000000000 ) ) ;
#810 = DIRECTION ( 'NONE',  ( 0.000000000000000000, 0.000000000000000000, 1.000000000000000000 ) ) ;
#811 = ORIENTED_EDGE ( 'NONE', *, *, #4867, .T. ) ;
#812 = ORIENTED_EDGE ( 'NONE', *, *, #4653, .T. ) ;
#813 = ORIENTED_EDGE ( 'NONE', *, *, #1830, .T. ) ;
#814 = AXIS2_PLACEMENT_3D ( 'NONE', #2399, #6019, #1158 ) ;
#815 = MECHANICAL_DESIGN_GEOMETRIC_PRESENTATION_REPRESENTATION (  '', ( #2840 ), #574 ) ;
#816 = VERTEX_POINT ( 'NONE', #6283 ) ;
#817 = APPLICATION_CONTEXT ( 'automotive_design' ) ;
#818 = DIRECTION ( 'NONE',  ( 1.000000000000000000, 0.000000000000000000, 0.000000000000000000 ) ) ;
#819 = SURFACE_STYLE_FILL_AREA ( #2015 ) ;
#820 = SURFACE_STYLE_USAGE ( .BOTH. , #4962 ) ;
#821 = CARTESIAN_POINT ( 'NONE',  ( 0.000000000000000000, 0.000000000000000000, 10.00000000000000000 ) ) ;
#822 = AXIS2_PLACEMENT_3D ( 'NONE', #4914, #539, #5357 ) ;
#823 = AXIS2_PLACEMENT_3D ( 'NONE', #1004, #3418, #6495 ) ;
#824 = ORIENTED_EDGE ( 'NONE', *, *, #453, .T. ) ;
#825 = ORIENTED_EDGE ( 'NONE', *, *, #3237, .T. ) ;
#826 = UNCERTAINTY_MEASURE_WITH_UNIT (LENGTH_MEASURE( 1.000000000000000082E-05 ), #6861, 'distance_accuracy_value', 'NONE');
#827 = DIRECTION ( 'NONE',  ( -0.4999999999999918954, -0.8660254037844432595, 0.000000000000000000 ) ) ;
#828 = FILL_AREA_STYLE ('',( #863 ) ) ;
#829 = LINE ( 'NONE', #5048, #4387 ) ;
#830 = CIRCLE ( 'NONE', #3608, 150.0000000000000568 ) ;
#831 = CARTESIAN_POINT ( 'NONE',  ( 8.000000000000000000, -4.618802153517011178, -3.985468820183668104 ) ) ;
#832 = ORIENTED_EDGE ( 'NONE', *, *, #529, .T. ) ;
#833 = AXIS2_PLACEMENT_3D ( 'NONE', #7236, #1838, #4860 ) ;
#834 = CARTESIAN_POINT ( 'NONE',  ( 0.000000000000000000, 0.000000000000000000, 0.000000000000000000 ) ) ;
#835 = DIRECTION ( 'NONE',  ( -0.8571673007021121116, 0.000000000000000000, -0.5150380749100544886 ) ) ;
#836 = DIRECTION ( 'NONE',  ( -1.000000000000000000, 0.000000000000000000, 0.000000000000000000 ) ) ;
#837 = CARTESIAN_POINT ( 'NONE',  ( -1.728922298134113098E-15, 8.513302795252935035E-16, 13.00000000000000178 ) ) ;
#838 = ORIENTED_EDGE ( 'NONE', *, *, #4223, .T. ) ;
#839 = AXIS2_PLACEMENT_3D ( 'NONE', #2155, #4033, #5889 ) ;
#840 = DIRECTION ( 'NONE',  ( 1.000000000000000000, 0.000000000000000000, 0.000000000000000000 ) ) ;
#841 = DIRECTION ( 'NONE',  ( 0.000000000000000000, -1.000000000000000000, 0.000000000000000000 ) ) ;
#842 = VECTOR ( 'NONE', #3621, 1000.000000000000000 ) ;
#843 = EDGE_CURVE ( 'NONE', #4257, #3121, #4817, .T. ) ;
#844 = CARTESIAN_POINT ( 'NONE',  ( 8.000000000000000000, 1.572549600175620066, -4.631055444744868410 ) ) ;
#845 = DIRECTION ( 'NONE',  ( -0.000000000000000000, -0.000000000000000000, 1.000000000000000000 ) ) ;
#846 = APPLICATION_PROTOCOL_DEFINITION ( 'draft international standard', 'automotive_design', 1998, #817 ) ;
#847 = DIRECTION ( 'NONE',  ( 1.000000000000000000, 0.000000000000000000, 0.000000000000000000 ) ) ;
#848 = EDGE_LOOP ( 'NONE', ( #5860, #2174 ) ) ;
#849 = ORIENTED_EDGE ( 'NONE', *, *, #1091, .F. ) ;
#850 = AXIS2_PLACEMENT_3D ( 'NONE', #1636, #7199, #4826 ) ;
#851 = EDGE_LOOP ( 'NONE', ( #1261, #352, #7402, #945 ) ) ;
#852 = ADVANCED_FACE ( 'NONE', ( #869 ), #3838, .T. ) ;
#853 = ORIENTED_EDGE ( 'NONE', *, *, #3653, .F. ) ;
#854 = CARTESIAN_POINT ( 'NONE',  ( 279.9963296805736945, -6.714540835673234486E-12, -82.99999999999998579 ) ) ;
#855 = CARTESIAN_POINT ( 'NONE',  ( 0.000000000000000000, 0.000000000000000000, -119.9999999999999858 ) ) ;
#856 = AXIS2_PLACEMENT_3D ( 'NONE', #4623, #4027, #1625 ) ;
#857 = DIRECTION ( 'NONE',  ( 0.000000000000000000, 0.000000000000000000, 1.000000000000000000 ) ) ;
#858 = ORIENTED_EDGE ( 'NONE', *, *, #4809, .F. ) ;
#859 = VECTOR ( 'NONE', #5866, 1000.000000000000000 ) ;
#860 = ORIENTED_EDGE ( 'NONE', *, *, #2548, .F. ) ;
#861 = DIRECTION ( 'NONE',  ( 1.000000000000000000, 0.000000000000000000, -0.000000000000000000 ) ) ;
#862 = ADVANCED_FACE ( 'NONE', ( #5018 ), #5492, .T. ) ;
#863 = FILL_AREA_STYLE_COLOUR ( '', #808 ) ;
#864 = CYLINDRICAL_SURFACE ( 'NONE', #2265, 32.81578194438969120 ) ;
#865 = CARTESIAN_POINT ( 'NONE',  ( -6.873268260756527152E-15, 0.000000000000000000, -79.99999999999995737 ) ) ;
#866 = DIRECTION ( 'NONE',  ( 0.000000000000000000, 0.000000000000000000, -1.000000000000000000 ) ) ;
#867 = ORIENTED_EDGE ( 'NONE', *, *, #6490, .T. ) ;
#868 = VECTOR ( 'NONE', #5469, 1000.000000000000000 ) ;
#869 = FACE_OUTER_BOUND ( 'NONE', #5970, .T. ) ;
#870 = DIRECTION ( 'NONE',  ( -1.000000000000000000, 0.000000000000000000, 0.000000000000000000 ) ) ;
#871 = CARTESIAN_POINT ( 'NONE',  ( -145.1064334105735725, 38.00161816110974655, 0.000000000000000000 ) ) ;
#872 = AXIS2_PLACEMENT_3D ( 'NONE', #6824, #1256, #1293 ) ;
#873 = CARTESIAN_POINT ( 'NONE',  ( 0.000000000000000000, 0.000000000000000000, -4.700000000000000178 ) ) ;
#874 = ORIENTED_EDGE ( 'NONE', *, *, #1580, .T. ) ;
#875 = DIRECTION ( 'NONE',  ( -0.000000000000000000, -0.000000000000000000, 1.000000000000000000 ) ) ;
#876 = CARTESIAN_POINT ( 'NONE',  ( 0.000000000000000000, 0.000000000000000000, -50.00000000000000000 ) ) ;
#877 = CARTESIAN_POINT ( 'NONE',  ( -5.238334947888650284, -36.57199107895616663, -3.000000000000000000 ) ) ;
#878 = EDGE_CURVE ( 'NONE', #5239, #4532, #709, .T. ) ;
#879 = CARTESIAN_POINT ( 'NONE',  ( 5.459126460941064352, -34.89491303563345070, -3.000000000000000000 ) ) ;
#880 = CARTESIAN_POINT ( 'NONE',  ( 8.000000000000000000, -4.618802153517012066, -4.700000000000000178 ) ) ;
#881 = PRODUCT_CONTEXT ( 'NONE', #6213, 'mechanical' ) ;
#882 = DIRECTION ( 'NONE',  ( 0.000000000000000000, 0.000000000000000000, 1.000000000000000000 ) ) ;
#883 = AXIS2_PLACEMENT_3D ( 'NONE', #1655, #1745, #6464 ) ;
#884 = ORIENTED_EDGE ( 'NONE', *, *, #2648, .F. ) ;
#885 = ORIENTED_EDGE ( 'NONE', *, *, #632, .F. ) ;
#886 = VERTEX_POINT ( 'NONE', #1504 ) ;
#887 = VERTEX_POINT ( 'NONE', #3911 ) ;
#888 = ORIENTED_EDGE ( 'NONE', *, *, #4171, .F. ) ;
#889 = AXIS2_PLACEMENT_3D ( 'NONE', #4293, #7335, #1330 ) ;
#890 = ADVANCED_FACE ( 'NONE', ( #513 ), #3951, .F. ) ;
#891 = FACE_OUTER_BOUND ( 'NONE', #5087, .T. ) ;
#892 = CYLINDRICAL_SURFACE ( 'NONE', #1896, 4.250000000000000000 ) ;
#893 = DIRECTION ( 'NONE',  ( -0.000000000000000000, -0.000000000000000000, 1.000000000000000000 ) ) ;
#894 = EDGE_CURVE ( 'NONE', #5165, #4732, #5114, .T. ) ;
#895 = EDGE_CURVE ( 'NONE', #6664, #1974, #7265, .T. ) ;
#896 = ORIENTED_EDGE ( 'NONE', *, *, #1918, .T. ) ;
#897 = EDGE_CURVE ( 'NONE', #5940, #2183, #5745, .T. ) ;
#898 = ORIENTED_EDGE ( 'NONE', *, *, #1531, .T. ) ;
#899 = ORIENTED_EDGE ( 'NONE', *, *, #4517, .T. ) ;
#900 = DIRECTION ( 'NONE',  ( 1.000000000000000000, 0.000000000000000000, 0.000000000000000000 ) ) ;
#901 = ADVANCED_FACE ( 'NONE', ( #434 ), #6948, .F. ) ;
#902 = DIRECTION ( 'NONE',  ( 1.000000000000000000, 0.000000000000000000, 0.000000000000000000 ) ) ;
#903 = CARTESIAN_POINT ( 'NONE',  ( -63.76644452187067458, 49.96174644486002592, 0.000000000000000000 ) ) ;
#904 = ORIENTED_EDGE ( 'NONE', *, *, #5478, .F. ) ;
#905 = EDGE_CURVE ( 'NONE', #5391, #738, #477, .T. ) ;
#906 = AXIS2_PLACEMENT_3D ( 'NONE', #3438, #5806, #391 ) ;
#907 = CARTESIAN_POINT ( 'NONE',  ( 114.7481648402866625, 207.8429183184022122, -120.0000000000000000 ) ) ;
#908 = CYLINDRICAL_SURFACE ( 'NONE', #3452, 30.00000000000000000 ) ;
#909 = DIRECTION ( 'NONE',  ( -0.000000000000000000, -0.000000000000000000, -1.000000000000000000 ) ) ;
#910 = AXIS2_PLACEMENT_3D ( 'NONE', #1832, #6638, #1226 ) ;
#911 = VECTOR ( 'NONE', #4475, 1000.000000000000000 ) ;
#912 = DIRECTION ( 'NONE',  ( -0.000000000000000000, -0.000000000000000000, 1.000000000000000000 ) ) ;
#913 = VERTEX_POINT ( 'NONE', #2307 ) ;
#914 =( REPRESENTATION_RELATIONSHIP ('NONE','NONE', #1229, #7725 ) REPRESENTATION_RELATIONSHIP_WITH_TRANSFORMATION ( #6057 )SHAPE_REPRESENTATION_RELATIONSHIP( ) );
#915 = CARTESIAN_POINT ( 'NONE',  ( 28.05900627794856206, 4.994213320838721160, -79.99999999999995737 ) ) ;
#916 = AXIS2_PLACEMENT_3D ( 'NONE', #6341, #927, #3343 ) ;
#917 = FACE_OUTER_BOUND ( 'NONE', #7070, .T. ) ;
#918 = FACE_OUTER_BOUND ( 'NONE', #7720, .T. ) ;
#919 = LINE ( 'NONE', #211, #3515 ) ;
#920 = PLANE ( 'NONE',  #7393 ) ;
#921 = DIRECTION ( 'NONE',  ( 3.081487911019577365E-33, -2.775557561562891967E-17, -1.000000000000000000 ) ) ;
#922 = AXIS2_PLACEMENT_3D ( 'NONE', #6154, #4808, #39 ) ;
#923 = ORIENTED_EDGE ( 'NONE', *, *, #5811, .F. ) ;
#924 = VERTEX_POINT ( 'NONE', #7571 ) ;
#925 = ORIENTED_EDGE ( 'NONE', *, *, #1091, .T. ) ;
#926 = VERTEX_POINT ( 'NONE', #5882 ) ;
#927 = DIRECTION ( 'NONE',  ( 0.000000000000000000, 0.000000000000000000, 1.000000000000000000 ) ) ;
#928 = VECTOR ( 'NONE', #3765, 1000.000000000000114 ) ;
#929 = DIRECTION ( 'NONE',  ( 0.3566035499204626702, -0.9342558044690565389, 2.649161120199466423E-17 ) ) ;
#930 = FACE_OUTER_BOUND ( 'NONE', #1696, .T. ) ;
#931 = DIRECTION ( 'NONE',  ( 0.000000000000000000, 0.000000000000000000, 1.000000000000000000 ) ) ;
#932 = CARTESIAN_POINT ( 'NONE',  ( 199.9963296805737230, -4.796075449120964792E-12, -50.00000000000004263 ) ) ;
#933 = ORIENTED_EDGE ( 'NONE', *, *, #2159, .T. ) ;
#934 = PRESENTATION_LAYER_ASSIGNMENT (  '', '', ( #180 ) ) ;
#935 = EDGE_CURVE ( 'NONE', #887, #5491, #2493, .T. ) ;
#936 = ORIENTED_EDGE ( 'NONE', *, *, #5900, .T. ) ;
#937 = ORIENTED_EDGE ( 'NONE', *, *, #5766, .F. ) ;
#938 = EDGE_CURVE ( 'NONE', #2235, #5183, #3616, .T. ) ;
#939 = CARTESIAN_POINT ( 'NONE',  ( 29.99999999999999289, 0.000000000000000000, -139.9999999999999716 ) ) ;
#940 =( NAMED_UNIT ( * ) SI_UNIT ( $, .STERADIAN. ) SOLID_ANGLE_UNIT ( ) );
#941 = AXIS2_PLACEMENT_3D ( 'NONE', #6424, #5826, #5272 ) ;
#942 = ADVANCED_FACE ( 'NONE', ( #4578 ), #355, .T. ) ;
#943 = DIRECTION ( 'NONE',  ( 1.000000000000000000, 0.000000000000000000, 0.000000000000000000 ) ) ;
#944 = DIRECTION ( 'NONE',  ( 1.000000000000000000, 0.000000000000000000, 0.000000000000000000 ) ) ;
#945 = ORIENTED_EDGE ( 'NONE', *, *, #5584, .T. ) ;
#946 = EDGE_CURVE ( 'NONE', #2474, #3424, #4485, .T. ) ;
#947 = CARTESIAN_POINT ( 'NONE',  ( -2.081668171172168513E-14, -9.237604307034017026, -3.985468820183668104 ) ) ;
#948 = CARTESIAN_POINT ( 'NONE',  ( -29.99999999999999289, 3.673940397442058389E-15, -122.9999999999999716 ) ) ;
#949 = AXIS2_PLACEMENT_3D ( 'NONE', #2122, #1512, #209 ) ;
#950 = CARTESIAN_POINT ( 'NONE',  ( -4.665299213380365018, 29.63502966507090619, -139.9999999999999716 ) ) ;
#951 = FACE_OUTER_BOUND ( 'NONE', #7184, .T. ) ;
#952 = VERTEX_POINT ( 'NONE', #1020 ) ;
#953 = AXIS2_PLACEMENT_3D ( 'NONE', #5493, #7311, #4822 ) ;
#954 = LINE ( 'NONE', #522, #5751 ) ;
#955 = DIRECTION ( 'NONE',  ( -0.000000000000000000, 0.000000000000000000, -1.000000000000000000 ) ) ;
#956 = PLANE ( 'NONE',  #1181 ) ;
#957 = DIRECTION ( 'NONE',  ( 0.000000000000000000, 0.000000000000000000, 1.000000000000000000 ) ) ;
#958 = CARTESIAN_POINT ( 'NONE',  ( 2.750000000000000000, -33.63777638310832430, -3.000000000000000000 ) ) ;
#959 = AXIS2_PLACEMENT_3D ( 'NONE', #4354, #6771, #1592 ) ;
#960 = DIRECTION ( 'NONE',  ( 5.551115123125782702E-17, 0.000000000000000000, 1.000000000000000000 ) ) ;
#961 = ORIENTED_EDGE ( 'NONE', *, *, #1772, .T. ) ;
#962 = EDGE_LOOP ( 'NONE', ( #3910, #335 ) ) ;
#963 = ORIENTED_EDGE ( 'NONE', *, *, #7549, .T. ) ;
#964 = AXIS2_PLACEMENT_3D ( 'NONE', #6067, #143, #1920 ) ;
#965 = CARTESIAN_POINT ( 'NONE',  ( -4.432034252711344102, 28.15327818181735964, -82.99999999999995737 ) ) ;
#966 = CARTESIAN_POINT ( 'NONE',  ( 3.200000000000008171, 0.000000000000000000, 0.000000000000000000 ) ) ;
#967 = CARTESIAN_POINT ( 'NONE',  ( 6.689127551062004962, 5.375634714784620627, -0.3173508448886543931 ) ) ;
#968 = FACE_OUTER_BOUND ( 'NONE', #763, .T. ) ;
#969 = DIRECTION ( 'NONE',  ( -1.000000000000000000, 0.000000000000000000, 0.000000000000000000 ) ) ;
#970 = AXIS2_PLACEMENT_3D ( 'NONE', #3411, #7665, #488 ) ;
#971 = ORIENTED_EDGE ( 'NONE', *, *, #5971, .T. ) ;
#972 = ORIENTED_EDGE ( 'NONE', *, *, #2975, .F. ) ;
#973 = ORIENTED_EDGE ( 'NONE', *, *, #1738, .F. ) ;
#974 = AXIS2_PLACEMENT_3D ( 'NONE', #1068, #986, #3480 ) ;
#975 = CARTESIAN_POINT ( 'NONE',  ( 0.000000000000000000, 0.000000000000000000, 0.000000000000000000 ) ) ;
#976 = CARTESIAN_POINT ( 'NONE',  ( 26.26644452187122170, -80.83980388508783221, 0.000000000000000000 ) ) ;
#977 = PRODUCT_RELATED_PRODUCT_CATEGORY ( 'part', '', ( #6750 ) ) ;
#978 = AXIS2_PLACEMENT_3D ( 'NONE', #4718, #5233, #4007 ) ;
#979 = CARTESIAN_POINT ( 'NONE',  ( 3.318518101603007864, 7.321656987762870550, 4.845028458294597151E-15 ) ) ;
#980 = VERTEX_POINT ( 'NONE', #4100 ) ;
#981 = AXIS2_PLACEMENT_3D ( 'NONE', #197, #6831, #1415 ) ;
#982 = EDGE_CURVE ( 'NONE', #7003, #6794, #4107, .T. ) ;
#983 = CIRCLE ( 'NONE', #7538, 5.000000000000004441 ) ;
#984 = DIRECTION ( 'NONE',  ( 0.000000000000000000, 0.000000000000000000, 1.000000000000000000 ) ) ;
#985 = DIRECTION ( 'NONE',  ( 0.000000000000000000, 0.000000000000000000, 1.000000000000000000 ) ) ;
#986 = DIRECTION ( 'NONE',  ( 0.000000000000000000, 0.000000000000000000, 1.000000000000000000 ) ) ;
#987 = CARTESIAN_POINT ( 'NONE',  ( -8.000000000000000000, -4.618802153517013842, -3.985468820183668104 ) ) ;
#988 = EDGE_CURVE ( 'NONE', #1789, #1868, #7640, .T. ) ;
#989 = VERTEX_POINT ( 'NONE', #7694 ) ;
#990 = AXIS2_PLACEMENT_3D ( 'NONE', #4722, #1412, #6541 ) ;
#991 = EDGE_CURVE ( 'NONE', #5791, #3509, #1093, .T. ) ;
#992 = CYLINDRICAL_SURFACE ( 'NONE', #1860, 5.000000000000000888 ) ;
#993 = AXIS2_PLACEMENT_3D ( 'NONE', #7133, #4168, #3502 ) ;
#994 = DIRECTION ( 'NONE',  ( -0.000000000000000000, -0.000000000000000000, -1.000000000000000000 ) ) ;
#995 = CARTESIAN_POINT ( 'NONE',  ( -68.76644452187068168, 49.96174644486002592, 0.000000000000000000 ) ) ;
#996 = CARTESIAN_POINT ( 'NONE',  ( -3.200000000000008171, 0.000000000000000000, 0.000000000000000000 ) ) ;
#997 = EDGE_CURVE ( 'NONE', #4531, #688, #3115, .T. ) ;
#998 = DIRECTION ( 'NONE',  ( -0.000000000000000000, -0.000000000000000000, -1.000000000000000000 ) ) ;
#999 = EDGE_LOOP ( 'NONE', ( #3310, #3719, #5793, #4925 ) ) ;
#1000 = ORIENTED_EDGE ( 'NONE', *, *, #5715, .F. ) ;
#1001 = CIRCLE ( 'NONE', #7678, 4.250000000000000000 ) ;
#1002 = ORIENTED_EDGE ( 'NONE', *, *, #4941, .F. ) ;
#1003 = EDGE_CURVE ( 'NONE', #3123, #7368, #6511, .T. ) ;
#1004 = CARTESIAN_POINT ( 'NONE',  ( -1.728922298134113098E-15, 8.513302795252935035E-16, 13.00000000000000178 ) ) ;
#1005 = CARTESIAN_POINT ( 'NONE',  ( -63.76644452187068879, 49.96174644486002592, -64.17200000000001125 ) ) ;
#1006 = CARTESIAN_POINT ( 'NONE',  ( -10.00000000000000000, 0.000000000000000000, 10.00000000000000000 ) ) ;
#1007 = DIRECTION ( 'NONE',  ( 1.000000000000000000, 0.000000000000000000, 0.000000000000000000 ) ) ;
#1008 = CIRCLE ( 'NONE', #134, 29.99999999999999289 ) ;
#1009 = CARTESIAN_POINT ( 'NONE',  ( 4.494751301858288528, -36.47409643479112162, -3.000000000000000000 ) ) ;
#1010 = CARTESIAN_POINT ( 'NONE',  ( 0.000000000000000000, 1.484218055610305731, -3.000000000000000000 ) ) ;
#1011 = ORIENTED_EDGE ( 'NONE', *, *, #3168, .F. ) ;
#1012 = ORIENTED_EDGE ( 'NONE', *, *, #122, .T. ) ;
#1013 = AXIS2_PLACEMENT_3D ( 'NONE', #629, #4330, #150 ) ;
#1014 = ORIENTED_EDGE ( 'NONE', *, *, #6400, .T. ) ;
#1015 = DIRECTION ( 'NONE',  ( -0.000000000000000000, -0.000000000000000000, 1.000000000000000000 ) ) ;
#1016 =( NAMED_UNIT ( * ) PLANE_ANGLE_UNIT ( ) SI_UNIT ( $, .RADIAN. ) );
#1017 = CARTESIAN_POINT ( 'NONE',  ( -129.9038105676659995, 74.99999999999971578, 10.00000000000000000 ) ) ;
#1018 = DIRECTION ( 'NONE',  ( -0.000000000000000000, -0.000000000000000000, -1.000000000000000000 ) ) ;
#1019 = ORIENTED_EDGE ( 'NONE', *, *, #5521, .F. ) ;
#1020 = CARTESIAN_POINT ( 'NONE',  ( -5.554394503829287011, 27.95350964898380752, -79.99999999999995737 ) ) ;
#1021 = LINE ( 'NONE', #1705, #4153 ) ;
#1022 = CARTESIAN_POINT ( 'NONE',  ( 2.645508037661878920, 7.710219529346608702, -4.631901280394570719 ) ) ;
#1023 = DIRECTION ( 'NONE',  ( 1.000000000000000000, 0.000000000000000000, 0.000000000000000000 ) ) ;
#1024 = AXIS2_PLACEMENT_3D ( 'NONE', #7353, #6917, #1352 ) ;
#1025 = VERTEX_POINT ( 'NONE', #7652 ) ;
#1026 = VERTEX_POINT ( 'NONE', #947 ) ;
#1027 = EDGE_CURVE ( 'NONE', #5335, #5921, #6769, .T. ) ;
#1028 = DIRECTION ( 'NONE',  ( 0.01999999999999999001, -0.9997999799959990108, 0.000000000000000000 ) ) ;
#1029 = LINE ( 'NONE', #5298, #7628 ) ;
#1030 = ADVANCED_FACE ( 'NONE', ( #7613 ), #2230, .F. ) ;
#1031 = CIRCLE ( 'NONE', #397, 5.000000000000004441 ) ;
#1032 = EDGE_CURVE ( 'NONE', #7478, #6571, #4999, .T. ) ;
#1033 = CARTESIAN_POINT ( 'NONE',  ( -68.76644452187068168, 49.96174644486002592, -64.17200000000001125 ) ) ;
#1034 = EDGE_LOOP ( 'NONE', ( #2693, #2711, #5172, #4955 ) ) ;
#1035 = DIRECTION ( 'NONE',  ( 0.9958843993404035144, -0.09063257223759993431, 0.000000000000000000 ) ) ;
#1036 = CARTESIAN_POINT ( 'NONE',  ( -350.0000000000000000, 300.0000000000001137, -82.99999999999998579 ) ) ;
#1037 = ITEM_DEFINED_TRANSFORMATION ( 'NONE', 'NONE', #3851,  #7485 ) ;
#1038 = ADVANCED_FACE ( 'NONE', ( #4142 ), #554, .T. ) ;
#1039 = CARTESIAN_POINT ( 'NONE',  ( -4.432034252711344102, 28.15327818181735964, -79.99999999999995737 ) ) ;
#1040 = ORIENTED_EDGE ( 'NONE', *, *, #1788, .T. ) ;
#1041 = ORIENTED_EDGE ( 'NONE', *, *, #1937, .F. ) ;
#1042 = AXIS2_PLACEMENT_3D ( 'NONE', #3660, #3625, #3111 ) ;
#1043 = VERTEX_POINT ( 'NONE', #5371 ) ;
#1044 = ADVANCED_FACE ( 'NONE', ( #1431 ), #3848, .F. ) ;
#1045 = CARTESIAN_POINT ( 'NONE',  ( -2.644994884459110907, 7.710515798486362371, -4.617753204360286468 ) ) ;
#1046 = DIRECTION ( 'NONE',  ( -0.000000000000000000, -0.000000000000000000, 1.000000000000000000 ) ) ;
#1047 = DIRECTION ( 'NONE',  ( -3.081487911019577365E-33, 2.775557561562891967E-17, 1.000000000000000000 ) ) ;
#1048 = DIRECTION ( 'NONE',  ( 0.9237280213470682178, 0.3830490080632377725, 0.000000000000000000 ) ) ;
#1049 = VECTOR ( 'NONE', #6193, 1000.000000000000000 ) ;
#1050 = DIRECTION ( 'NONE',  ( -0.000000000000000000, -0.000000000000000000, 1.000000000000000000 ) ) ;
#1051 = VERTEX_POINT ( 'NONE', #6214 ) ;
#1052 = ADVANCED_BREP_SHAPE_REPRESENTATION ( '', ( #5741, #7485 ), #6116 ) ;
#1053 = VERTEX_POINT ( 'NONE', #5653 ) ;
#1054=STYLED_ITEM('',(#7823),#5726);
#1055 = AXIS2_PLACEMENT_3D ( 'NONE', #2477, #1994, #6680 ) ;
#1056 = ORIENTED_EDGE ( 'NONE', *, *, #7068, .F. ) ;
#1057 = CARTESIAN_POINT ( 'NONE',  ( 10.16320117273318679, -26.62629042736811869, -122.9999999999999716 ) ) ;
#1058 = FILL_AREA_STYLE_COLOUR ( '', #127 ) ;
#1059 = SURFACE_SIDE_STYLE ('',( #507 ) ) ;
#1060 = CYLINDRICAL_SURFACE ( 'NONE', #6349, 40.00000000000000711 ) ;
#1061 = AXIS2_PLACEMENT_3D ( 'NONE', #6484, #7155, #7343 ) ;
#1062 = CARTESIAN_POINT ( 'NONE',  ( 0.7499999999999730216, -37.49249924984995630, -3.000000000000000000 ) ) ;
#1063 = EDGE_LOOP ( 'NONE', ( #4829, #3062, #2505, #4842 ) ) ;
#1064 = CIRCLE ( 'NONE', #5224, 32.81578194438969120 ) ;
#1065 = CARTESIAN_POINT ( 'NONE',  ( -129.9038105676659995, 74.99999999999971578, 0.000000000000000000 ) ) ;
#1066 = FACE_BOUND ( 'NONE', #2917, .T. ) ;
#1067 =( REPRESENTATION_RELATIONSHIP ('NONE','NONE', #1229, #1433 ) REPRESENTATION_RELATIONSHIP_WITH_TRANSFORMATION ( #4906 )SHAPE_REPRESENTATION_RELATIONSHIP( ) );
#1068 = CARTESIAN_POINT ( 'NONE',  ( 0.000000000000000000, 0.000000000000000000, 0.000000000000000000 ) ) ;
#1069 = FACE_OUTER_BOUND ( 'NONE', #6626, .T. ) ;
#1070 = ORIENTED_EDGE ( 'NONE', *, *, #3698, .T. ) ;
#1071 = ORIENTED_EDGE ( 'NONE', *, *, #5323, .F. ) ;
#1072 = CYLINDRICAL_SURFACE ( 'NONE', #5378, 32.81578194438969120 ) ;
#1073 =( GEOMETRIC_REPRESENTATION_CONTEXT ( 3 ) GLOBAL_UNCERTAINTY_ASSIGNED_CONTEXT ( ( #4788 ) ) GLOBAL_UNIT_ASSIGNED_CONTEXT ( ( #5810, #396, #4629 ) ) REPRESENTATION_CONTEXT ( 'NONE', 'WORKASPACE' ) );
#1074 = DIRECTION ( 'NONE',  ( 1.000000000000000000, 0.000000000000000000, 0.000000000000000000 ) ) ;
#1075 = CARTESIAN_POINT ( 'NONE',  ( -119.9981648402868046, 207.8429183184021554, -8.673617379884035472E-15 ) ) ;
#1076 = CARTESIAN_POINT ( 'NONE',  ( -10.00000000000000000, 0.000000000000000000, -60.00000000000000711 ) ) ;
#1077 = CARTESIAN_POINT ( 'NONE',  ( 8.000000000000000000, 4.618802153517004072, -4.700000000000000178 ) ) ;
#1078 = ITEM_DEFINED_TRANSFORMATION ( 'NONE', 'NONE', #2589,  #7485 ) ;
#1079 = FACE_OUTER_BOUND ( 'NONE', #670, .T. ) ;
#1080 = ORIENTED_EDGE ( 'NONE', *, *, #2057, .T. ) ;
#1081 = AXIS2_PLACEMENT_3D ( 'NONE', #4060, #5924, #4025 ) ;
#1082 = ORIENTED_EDGE ( 'NONE', *, *, #1569, .T. ) ;
#1083 = ORIENTED_EDGE ( 'NONE', *, *, #6074, .T. ) ;
#1084 = EDGE_CURVE ( 'NONE', #2183, #6897, #6251, .T. ) ;
#1085 = CARTESIAN_POINT ( 'NONE',  ( 6.689127551062004962, 5.375634714784622403, -4.382649155111347561 ) ) ;
#1086 = CIRCLE ( 'NONE', #2109, 37.49999999999997868 ) ;
#1087 = DIRECTION ( 'NONE',  ( -0.000000000000000000, -0.000000000000000000, 1.000000000000000000 ) ) ;
#1088 = DIRECTION ( 'NONE',  ( 1.000000000000000000, 0.000000000000000000, 0.000000000000000000 ) ) ;
#1089 = DIRECTION ( 'NONE',  ( 0.000000000000000000, 0.000000000000000000, 1.000000000000000000 ) ) ;
#1090 = CARTESIAN_POINT ( 'NONE',  ( 6.686525924292793022, -5.377136764700165550, -0.3167204509598423590 ) ) ;
#1091 = EDGE_CURVE ( 'NONE', #5886, #6942, #3740, .T. ) ;
#1092 = ORIENTED_EDGE ( 'NONE', *, *, #3497, .T. ) ;
#1093 = CIRCLE ( 'NONE', #5251, 150.0000000000000568 ) ;
#1094 = ORIENTED_EDGE ( 'NONE', *, *, #3440, .F. ) ;
#1095 = VERTEX_POINT ( 'NONE', #7429 ) ;
#1096 = DIRECTION ( 'NONE',  ( -1.000000000000000000, 0.000000000000000000, 0.000000000000000000 ) ) ;
#1097 = SURFACE_STYLE_FILL_AREA ( #4770 ) ;
#1098 = CIRCLE ( 'NONE', #5510, 29.99999999999999289 ) ;
#1099 = LINE ( 'NONE', #1749, #2193 ) ;
#1100 = FACE_BOUND ( 'NONE', #7449, .T. ) ;
#1101 = ORIENTED_EDGE ( 'NONE', *, *, #4523, .F. ) ;
#1102 = VERTEX_POINT ( 'NONE', #6177 ) ;
#1103 = AXIS2_PLACEMENT_3D ( 'NONE', #5937, #2278, #2945 ) ;
#1104 = ADVANCED_FACE ( 'NONE', ( #208 ), #3770, .F. ) ;
#1105 = DIRECTION ( 'NONE',  ( 0.9412010056177179118, 0.3378471059875997051, 0.000000000000000000 ) ) ;
#1106 = CARTESIAN_POINT ( 'NONE',  ( -6.873268260756527152E-15, 0.000000000000000000, -79.99999999999995737 ) ) ;
#1107 = CARTESIAN_POINT ( 'NONE',  ( 3.500000000000006661, 0.000000000000000000, -31.52499999999999858 ) ) ;
#1108 = CARTESIAN_POINT ( 'NONE',  ( -29.99999999999999289, 3.673940397442058389E-15, 10.00000000000000888 ) ) ;
#1109 = EDGE_LOOP ( 'NONE', ( #3754, #7137 ) ) ;
#1110 = ORIENTED_EDGE ( 'NONE', *, *, #2750, .T. ) ;
#1111 = CIRCLE ( 'NONE', #7411, 10.00000000000000178 ) ;
#1112 = FACE_BOUND ( 'NONE', #2728, .T. ) ;
#1113 = FACE_OUTER_BOUND ( 'NONE', #4887, .T. ) ;
#1114 = DIRECTION ( 'NONE',  ( 0.000000000000000000, 0.000000000000000000, -1.000000000000000000 ) ) ;
#1115 = FACE_BOUND ( 'NONE', #1109, .T. ) ;
#1116 = CARTESIAN_POINT ( 'NONE',  ( -3.500000000000007550, 0.000000000000000000, -30.30000000000000071 ) ) ;
#1117 = ITEM_DEFINED_TRANSFORMATION ( 'NONE', 'NONE', #7618,  #7485 ) ;
#1118 = CONICAL_SURFACE ( 'NONE', #5529, 8.000000000000000000, 1.047197551196596299 ) ;
#1119 = CARTESIAN_POINT ( 'NONE',  ( -28.05900627794857272, -4.994213320838722936, -79.99999999999995737 ) ) ;
#1120 = VERTEX_POINT ( 'NONE', #1473 ) ;
#1121 = VERTEX_POINT ( 'NONE', #2665 ) ;
#1122 = ORIENTED_EDGE ( 'NONE', *, *, #7750, .F. ) ;
#1123 = AXIS2_PLACEMENT_3D ( 'NONE', #6696, #67, #6816 ) ;
#1124 = CARTESIAN_POINT ( 'NONE',  ( -7.039801714450301422E-15, 0.000000000000000000, -82.99999999999995737 ) ) ;
#1125 = CARTESIAN_POINT ( 'NONE',  ( -63.51644452187023404, -49.96174644486060856, 0.000000000000000000 ) ) ;
#1126 = LINE ( 'NONE', #4642, #3627 ) ;
#1127 = DIRECTION ( 'NONE',  ( -0.8090169943749422332, -0.5877852522924802425, 0.000000000000000000 ) ) ;
#1128 = CARTESIAN_POINT ( 'NONE',  ( 5.354491962338128630, -6.146186931204413284, -0.06809871960543142921 ) ) ;
#1129 = VECTOR ( 'NONE', #4406, 1000.000000000000000 ) ;
#1130 = ORIENTED_EDGE ( 'NONE', *, *, #6583, .T. ) ;
#1131 = ORIENTED_EDGE ( 'NONE', *, *, #5478, .T. ) ;
#1132 = ADVANCED_FACE ( 'NONE', ( #766 ), #5138, .T. ) ;
#1133 = EDGE_LOOP ( 'NONE', ( #5984, #5197, #2414, #4649 ) ) ;
#1134 = AXIS2_PLACEMENT_3D ( 'NONE', #4260, #7227, #1827 ) ;
#1135 = DIRECTION ( 'NONE',  ( -1.000000000000000000, 1.586032892321652729E-16, 0.000000000000000000 ) ) ;
#1136 = DIRECTION ( 'NONE',  ( 1.000000000000000000, 0.000000000000000000, -0.000000000000000000 ) ) ;
#1137 = ADVANCED_FACE ( 'NONE', ( #2625, #7467, #3917, #2079, #325, #7391, #4472 ), #5581, .T. ) ;
#1138 = EDGE_CURVE ( 'NONE', #3181, #5886, #1999, .T. ) ;
#1139 = DIRECTION ( 'NONE',  ( -0.1555099737793451675, 0.9878343221690302212, -1.110223024625155986E-18 ) ) ;
#1140 = EDGE_CURVE ( 'NONE', #4191, #4160, #4986, .T. ) ;
#1141 = ORIENTED_EDGE ( 'NONE', *, *, #1629, .T. ) ;
#1142 = VECTOR ( 'NONE', #5553, 1000.000000000000000 ) ;
#1143 = VECTOR ( 'NONE', #1204, 1000.000000000000000 ) ;
#1144 = ADVANCED_FACE ( 'NONE', ( #1961 ), #1597, .T. ) ;
#1145 = DIRECTION ( 'NONE',  ( -0.000000000000000000, -0.000000000000000000, 1.000000000000000000 ) ) ;
#1146 = DIRECTION ( 'NONE',  ( 0.9845265360683707057, 0.1752355551171480841, 0.000000000000000000 ) ) ;
#1147 = DIRECTION ( 'NONE',  ( 0.000000000000000000, 0.000000000000000000, 1.000000000000000000 ) ) ;
#1148 = DIRECTION ( 'NONE',  ( 1.000000000000000000, 0.000000000000000000, 0.000000000000000000 ) ) ;
#1149 = ORIENTED_EDGE ( 'NONE', *, *, #1937, .T. ) ;
#1150 = ORIENTED_EDGE ( 'NONE', *, *, #705, .T. ) ;
#1151 = ORIENTED_EDGE ( 'NONE', *, *, #419, .F. ) ;
#1152 = FACE_OUTER_BOUND ( 'NONE', #1692, .T. ) ;
#1153 = CARTESIAN_POINT ( 'NONE',  ( -37.49999999999997868, 4.592425496802572000E-15, -90.00000000000000000 ) ) ;
#1154 =( NAMED_UNIT ( * ) SI_UNIT ( $, .STERADIAN. ) SOLID_ANGLE_UNIT ( ) );
#1155 = CARTESIAN_POINT ( 'NONE',  ( 0.000000000000000000, 0.000000000000000000, 0.000000000000000000 ) ) ;
#1156 = FACE_OUTER_BOUND ( 'NONE', #4453, .T. ) ;
#1157 = CIRCLE ( 'NONE', #1802, 5.250000000000004441 ) ;
#1158 = DIRECTION ( 'NONE',  ( 1.000000000000000000, 0.000000000000000000, -0.000000000000000000 ) ) ;
#1159 = EDGE_LOOP ( 'NONE', ( #4431, #1815 ) ) ;
#1160 = CIRCLE ( 'NONE', #7322, 150.0000000000000568 ) ;
#1161 = EDGE_LOOP ( 'NONE', ( #2545, #5550, #1660, #6503 ) ) ;
#1162 = CIRCLE ( 'NONE', #3063, 29.99999999999999289 ) ;
#1163 = DIRECTION ( 'NONE',  ( 0.000000000000000000, 0.000000000000000000, 1.000000000000000000 ) ) ;
#1164 = PLANE ( 'NONE',  #6663 ) ;
#1165 = FACE_OUTER_BOUND ( 'NONE', #7589, .T. ) ;
#1166 = DIRECTION ( 'NONE',  ( 0.000000000000000000, 0.000000000000000000, 1.000000000000000000 ) ) ;
#1167 = DIRECTION ( 'NONE',  ( 0.000000000000000000, 0.000000000000000000, 1.000000000000000000 ) ) ;
#1168 = CARTESIAN_POINT ( 'NONE',  ( 8.000000000000000000, -4.618802153517011178, -0.7145311798163319628 ) ) ;
#1169 = CONICAL_SURFACE ( 'NONE', #1042, 4.999999999999990230, 0.7853981633974482790 ) ;
#1170 = VERTEX_POINT ( 'NONE', #282 ) ;
#1171 = ORIENTED_EDGE ( 'NONE', *, *, #4898, .F. ) ;
#1172 =( REPRESENTATION_RELATIONSHIP ('NONE','NONE', #1229, #1433 ) REPRESENTATION_RELATIONSHIP_WITH_TRANSFORMATION ( #204 )SHAPE_REPRESENTATION_RELATIONSHIP( ) );
#1173 = EDGE_LOOP ( 'NONE', ( #97, #3739, #149, #5750, #3439, #1470 ) ) ;
#1174 = VECTOR ( 'NONE', #3724, 1000.000000000000000 ) ;
#1175 = DIRECTION ( 'NONE',  ( 1.000000000000000000, 0.000000000000000000, 0.000000000000000000 ) ) ;
#1176 = CARTESIAN_POINT ( 'NONE',  ( -8.000000000000001776, -3.098204225878171680, -0.3157906771918751465 ) ) ;
#1177 = DIRECTION ( 'NONE',  ( -0.000000000000000000, -0.000000000000000000, 1.000000000000000000 ) ) ;
#1178 = EDGE_CURVE ( 'NONE', #4200, #3050, #4365, .T. ) ;
#1179 = MECHANICAL_DESIGN_GEOMETRIC_PRESENTATION_REPRESENTATION (  '', ( #3832 ), #5212 ) ;
#1180 = ORIENTED_EDGE ( 'NONE', *, *, #4758, .F. ) ;
#1181 = AXIS2_PLACEMENT_3D ( 'NONE', #4034, #328, #5851 ) ;
#1182 = ORIENTED_EDGE ( 'NONE', *, *, #6944, .T. ) ;
#1183 = EDGE_CURVE ( 'NONE', #3506, #5913, #2614, .T. ) ;
#1184 = EDGE_CURVE ( 'NONE', #1401, #5872, #5501, .T. ) ;
#1185 = CARTESIAN_POINT ( 'NONE',  ( 0.000000000000000000, 0.000000000000000000, -82.99999999999998579 ) ) ;
#1186 = MECHANICAL_DESIGN_GEOMETRIC_PRESENTATION_REPRESENTATION (  '', ( #429 ), #6358 ) ;
#1187 = AXIS2_PLACEMENT_3D ( 'NONE', #1075, #5935, #4073 ) ;
#1188 = DIRECTION ( 'NONE',  ( 0.1305261922200541547, 0.9914448613738101601, 0.000000000000000000 ) ) ;
#1189 = CYLINDRICAL_SURFACE ( 'NONE', #910, 6.099504629071904382 ) ;
#1190 = ORIENTED_EDGE ( 'NONE', *, *, #3670, .T. ) ;
#1191 = VERTEX_POINT ( 'NONE', #2121 ) ;
#1192 = ADVANCED_FACE ( 'NONE', ( #6920 ), #5730, .F. ) ;
#1193 = AXIS2_PLACEMENT_3D ( 'NONE', #1638, #6488, #5857 ) ;
#1194 = VERTEX_POINT ( 'NONE', #6482 ) ;
#1195 = PRODUCT_DEFINITION_SHAPE ( 'NONE', 'NONE',  #7059 ) ;
#1196 = LINE ( 'NONE', #5321, #3108 ) ;
#1197 = DIRECTION ( 'NONE',  ( 0.000000000000000000, 0.000000000000000000, -1.000000000000000000 ) ) ;
#1198 = CARTESIAN_POINT ( 'NONE',  ( 0.000000000000000000, 0.000000000000000000, -109.9956969048621716 ) ) ;
#1199 = LINE ( 'NONE', #4350, #6780 ) ;
#1200 = ITEM_DEFINED_TRANSFORMATION ( 'NONE', 'NONE', #2844,  #7485 ) ;
#1201 = AXIS2_PLACEMENT_3D ( 'NONE', #7208, #6540, #6620 ) ;
#1202 = CARTESIAN_POINT ( 'NONE',  ( -4.250000000000000000, 5.204748896376250699E-16, -4.149444346342716194 ) ) ;
#1203 = ORIENTED_EDGE ( 'NONE', *, *, #2453, .F. ) ;
#1204 = DIRECTION ( 'NONE',  ( 1.000000000000000000, 0.000000000000000000, -0.000000000000000000 ) ) ;
#1205 = LINE ( 'NONE', #3620, #3011 ) ;
#1206 = DIRECTION ( 'NONE',  ( 0.000000000000000000, 0.000000000000000000, -1.000000000000000000 ) ) ;
#1207 = CARTESIAN_POINT ( 'NONE',  ( 119.9981648402867052, 207.8429183184022406, -124.7000000000000028 ) ) ;
#1208 = VECTOR ( 'NONE', #1074, 1000.000000000000000 ) ;
#1209 =( NAMED_UNIT ( * ) SI_UNIT ( $, .STERADIAN. ) SOLID_ANGLE_UNIT ( ) );
#1210 = CYLINDRICAL_SURFACE ( 'NONE', #993, 150.0000000000000568 ) ;
#1211 = EDGE_LOOP ( 'NONE', ( #888, #3113, #3835, #6079 ) ) ;
#1212 = VERTEX_POINT ( 'NONE', #4586 ) ;
#1213 = VECTOR ( 'NONE', #2509, 1000.000000000000000 ) ;
#1214 = ORIENTED_EDGE ( 'NONE', *, *, #988, .T. ) ;
#1215 = DIRECTION ( 'NONE',  ( 0.000000000000000000, -1.000000000000000000, 0.000000000000000000 ) ) ;
#1216 =( LENGTH_UNIT ( ) NAMED_UNIT ( * ) SI_UNIT ( .MILLI., .METRE. ) );
#1217 = LINE ( 'NONE', #4845, #1423 ) ;
#1218 = AXIS2_PLACEMENT_3D ( 'NONE', #5252, #388, #6471 ) ;
#1219 = VERTEX_POINT ( 'NONE', #7035 ) ;
#1220 = APPLICATION_CONTEXT ( 'automotive_design' ) ;
#1221 = ORIENTED_EDGE ( 'NONE', *, *, #7269, .F. ) ;
#1222 = AXIS2_PLACEMENT_3D ( 'NONE', #2444, #7326, #5503 ) ;
#1223 = PRODUCT_DEFINITION ( 'UNKNOWN', '', #2441, #6530 ) ;
#1224 = FACE_OUTER_BOUND ( 'NONE', #5370, .T. ) ;
#1225 = CARTESIAN_POINT ( 'NONE',  ( 0.000000000000000000, 0.000000000000000000, -4.700000000000000178 ) ) ;
#1226 = DIRECTION ( 'NONE',  ( 1.000000000000000000, 0.000000000000000000, 0.000000000000000000 ) ) ;
#1227 = ORIENTED_EDGE ( 'NONE', *, *, #6300, .F. ) ;
#1228 = B_SPLINE_CURVE_WITH_KNOTS ( 'NONE', 3,
 ( #3576, #4601, #2951, #7006, #7749, #6420 ),
 .UNSPECIFIED., .F., .F.,
 ( 4, 2, 4 ),
 ( 2.380731629626129180E-07, 0.002336973833157558137, 0.004673709593152153112 ),
 .UNSPECIFIED. ) ;
#1229 = SHAPE_REPRESENTATION ( 'MAS-196', ( #1295, #941, #2969, #4975, #5993, #2594, #6995, #2589, #3851, #4851, #439, #2481, #5230, #1451, #3472, #5610, #6871, #6625, #3596, #3220, #822, #5862, #4598, #4222, #192, #7618, #2225, #1201, #1843, #6243, #2844, #7253, #4942, #2936, #3938, #7464, #2809, #666, #6958, #3191 ), #1935 ) ;
#1230 = ORIENTED_EDGE ( 'NONE', *, *, #6643, .T. ) ;
#1231 = DIRECTION ( 'NONE',  ( 0.000000000000000000, 1.000000000000000000, 0.000000000000000000 ) ) ;
#1232 = CARTESIAN_POINT ( 'NONE',  ( 0.000000000000000000, 0.000000000000000000, -139.9999999999999716 ) ) ;
#1233 = AXIS2_PLACEMENT_3D ( 'NONE', #6332, #3600, #6598 ) ;
#1234 = DIRECTION ( 'NONE',  ( 1.000000000000000000, 0.000000000000000000, 0.000000000000000000 ) ) ;
#1235 = CARTESIAN_POINT ( 'NONE',  ( 32.81578194438969120, 1.484218055610305731, -3.000000000000000000 ) ) ;
#1236 = EDGE_CURVE ( 'NONE', #2058, #5637, #1988, .T. ) ;
#1237 = DIRECTION ( 'NONE',  ( 0.000000000000000000, 0.000000000000000000, 1.000000000000000000 ) ) ;
#1238 = VERTEX_POINT ( 'NONE', #2857 ) ;
#1239 = AXIS2_PLACEMENT_3D ( 'NONE', #4603, #2287, #7634 ) ;
#1240 = EDGE_CURVE ( 'NONE', #1722, #5462, #5754, .T. ) ;
#1241 = CARTESIAN_POINT ( 'NONE',  ( 0.000000000000000000, 0.000000000000000000, 10.00000000000000000 ) ) ;
#1242 = ADVANCED_FACE ( 'NONE', ( #1631 ), #5932, .T. ) ;
#1243 = B_SPLINE_CURVE_WITH_KNOTS ( 'NONE', 3,
 ( #2727, #2227, #3318, #4575, #979, #2147 ),
 .UNSPECIFIED., .F., .F.,
 ( 4, 2, 4 ),
 ( 2.380731629561858173E-07, 0.002336973833157559872, 0.004673709593152164388 ),
 .UNSPECIFIED. ) ;
#1244 = CARTESIAN_POINT ( 'NONE',  ( -68.76644452187024115, -49.96174644486060856, 0.000000000000000000 ) ) ;
#1245 = CARTESIAN_POINT ( 'NONE',  ( 1.469553684752138043E-14, 239.9963296805737230, 10.00000000000000000 ) ) ;
#1246 = DIRECTION ( 'NONE',  ( 0.000000000000000000, 0.000000000000000000, -1.000000000000000000 ) ) ;
#1247 = DIRECTION ( 'NONE',  ( 0.000000000000000000, 0.000000000000000000, -1.000000000000000000 ) ) ;
#1248 = CARTESIAN_POINT ( 'NONE',  ( 10.00000000000000000, 28.28427124746189136, 10.00000000000000888 ) ) ;
#1249 = CARTESIAN_POINT ( 'NONE',  ( 26.26644452187122170, -80.83980388508783221, 10.00000000000000000 ) ) ;
#1250 = ADVANCED_FACE ( 'NONE', ( #6954 ), #1072, .T. ) ;
#1251 = ORIENTED_EDGE ( 'NONE', *, *, #2890, .T. ) ;
#1252 = VECTOR ( 'NONE', #3777, 1000.000000000000000 ) ;
#1253 = EDGE_LOOP ( 'NONE', ( #3710, #461 ) ) ;
#1254 = EDGE_LOOP ( 'NONE', ( #4422, #6940 ) ) ;
#1255 = DIRECTION ( 'NONE',  ( -0.000000000000000000, -0.000000000000000000, 1.000000000000000000 ) ) ;
#1256 = DIRECTION ( 'NONE',  ( 0.000000000000000000, 0.000000000000000000, 1.000000000000000000 ) ) ;
#1257 = PRESENTATION_LAYER_ASSIGNMENT (  '', '', ( #3027 ) ) ;
#1258 = CARTESIAN_POINT ( 'NONE',  ( -29.99999999999999289, 3.673940397442058389E-15, 13.00000000000001066 ) ) ;
#1259 = PRODUCT_DEFINITION_SHAPE ( 'NONE', 'NONE',  #6003 ) ;
#1260 = ORIENTED_EDGE ( 'NONE', *, *, #5004, .F. ) ;
#1261 = ORIENTED_EDGE ( 'NONE', *, *, #3237, .F. ) ;
#1262 = AXIS2_PLACEMENT_3D ( 'NONE', #5714, #308, #4417 ) ;
#1263 = DIRECTION ( 'NONE',  ( -0.000000000000000000, -0.000000000000000000, -1.000000000000000000 ) ) ;
#1264 = DIRECTION ( 'NONE',  ( -1.000000000000000000, 2.398081733190337496E-14, 0.000000000000000000 ) ) ;
#1265 = CONICAL_SURFACE ( 'NONE', #3540, 8.000000000000000000, 1.047197551196596299 ) ;
#1266 = DIRECTION ( 'NONE',  ( 0.000000000000000000, 1.224646799147359124E-16, 1.000000000000000000 ) ) ;
#1267 = ORIENTED_EDGE ( 'NONE', *, *, #5379, .T. ) ;
#1268 = ORIENTED_EDGE ( 'NONE', *, *, #6226, .T. ) ;
#1269 = CIRCLE ( 'NONE', #1652, 4.171999999999995268 ) ;
#1270 = LINE ( 'NONE', #682, #7760 ) ;
#1271 = DIRECTION ( 'NONE',  ( 1.000000000000000000, 0.000000000000000000, 0.000000000000000000 ) ) ;
#1272 = PLANE ( 'NONE',  #4013 ) ;
#1273 = FACE_OUTER_BOUND ( 'NONE', #1702, .T. ) ;
#1274 = DIRECTION ( 'NONE',  ( 0.01999999999999999001, 0.9997999799959990108, -0.000000000000000000 ) ) ;
#1275 = EDGE_LOOP ( 'NONE', ( #7512, #1260, #4727, #6662 ) ) ;
#1276 = EDGE_CURVE ( 'NONE', #3299, #5007, #5850, .T. ) ;
#1277 = ADVANCED_FACE ( 'NONE', ( #3524, #1112, #4068 ), #2899, .F. ) ;
#1278 = EDGE_CURVE ( 'NONE', #2635, #6563, #954, .T. ) ;
#1279 = DIRECTION ( 'NONE',  ( 1.000000000000000000, 0.000000000000000000, 0.000000000000000000 ) ) ;
#1280 = ADVANCED_FACE ( 'NONE', ( #2778 ), #5770, .T. ) ;
#1281 = CARTESIAN_POINT ( 'NONE',  ( 0.000000000000000000, 0.000000000000000000, 3.859999999999999876 ) ) ;
#1282 = LINE ( 'NONE', #3774, #4249 ) ;
#1283 = DIRECTION ( 'NONE',  ( 0.000000000000000000, 0.000000000000000000, 1.000000000000000000 ) ) ;
#1284 =( NAMED_UNIT ( * ) PLANE_ANGLE_UNIT ( ) SI_UNIT ( $, .RADIAN. ) );
#1285 = LINE ( 'NONE', #696, #1252 ) ;
#1286 = CARTESIAN_POINT ( 'NONE',  ( 3.500000000000007550, 3.710679801416480038E-15, 30.30000000000000071 ) ) ;
#1287 = ORIENTED_EDGE ( 'NONE', *, *, #1958, .T. ) ;
#1288 = VECTOR ( 'NONE', #6880, 1000.000000000000000 ) ;
#1289 = EDGE_LOOP ( 'NONE', ( #5315, #2029, #3494, #4839 ) ) ;
#1290 = EDGE_CURVE ( 'NONE', #6532, #7160, #3619, .T. ) ;
#1291 = ORIENTED_EDGE ( 'NONE', *, *, #4755, .T. ) ;
#1292 = CARTESIAN_POINT ( 'NONE',  ( -10.00000000000000000, 42.00000000000000000, 0.000000000000000000 ) ) ;
#1293 = DIRECTION ( 'NONE',  ( 1.000000000000000000, 0.000000000000000000, 0.000000000000000000 ) ) ;
#1294 = FILL_AREA_STYLE_COLOUR ( '', #5225 ) ;
#1295 = AXIS2_PLACEMENT_3D ( 'NONE', #1987, #3202, #2613 ) ;
#1296 = DIRECTION ( 'NONE',  ( -0.000000000000000000, -0.000000000000000000, 1.000000000000000000 ) ) ;
#1297 = ORIENTED_EDGE ( 'NONE', *, *, #1032, .F. ) ;
#1298 = VERTEX_POINT ( 'NONE', #2939 ) ;
#1299 = CIRCLE ( 'NONE', #4697, 0.3000000000000016542 ) ;
#1300 = DIRECTION ( 'NONE',  ( 1.000000000000000000, 0.000000000000000000, 0.000000000000000000 ) ) ;
#1301 = CARTESIAN_POINT ( 'NONE',  ( 0.000000000000000000, 0.000000000000000000, 0.000000000000000000 ) ) ;
#1302 = CARTESIAN_POINT ( 'NONE',  ( -73.76644452187071010, 49.96174644486006855, -134.1720000000000255 ) ) ;
#1303 = AXIS2_PLACEMENT_3D ( 'NONE', #509, #1177, #469 ) ;
#1304 = LINE ( 'NONE', #4815, #2060 ) ;
#1305 = ORIENTED_EDGE ( 'NONE', *, *, #6977, .T. ) ;
#1306 = ORIENTED_EDGE ( 'NONE', *, *, #5427, .F. ) ;
#1307 = CIRCLE ( 'NONE', #4580, 1.250000000000000444 ) ;
#1308 = AXIS2_PLACEMENT_3D ( 'NONE', #285, #6411, #2158 ) ;
#1309 = CARTESIAN_POINT ( 'NONE',  ( -73.76644452187066747, 49.96174644486002592, -40.00000000000000000 ) ) ;
#1310 = DIRECTION ( 'NONE',  ( -1.000000000000000000, -8.881784197001252323E-16, 0.000000000000000000 ) ) ;
#1311 = CYLINDRICAL_SURFACE ( 'NONE', #45, 5.249999999999991118 ) ;
#1312 = CARTESIAN_POINT ( 'NONE',  ( 26.26644452187122170, -80.83980388508783221, 10.00000000000000000 ) ) ;
#1313 = UNCERTAINTY_MEASURE_WITH_UNIT (LENGTH_MEASURE( 1.000000000000000082E-05 ), #3527, 'distance_accuracy_value', 'NONE');
#1314 = LINE ( 'NONE', #5461, #3554 ) ;
#1315 = AXIS2_PLACEMENT_3D ( 'NONE', #7626, #4670, #6374 ) ;
#1316 = ORIENTED_EDGE ( 'NONE', *, *, #218, .F. ) ;
#1317 = CARTESIAN_POINT ( 'NONE',  ( -350.0000000000000000, 300.0000000000001137, -1041.954445729288636 ) ) ;
#1318 = DIRECTION ( 'NONE',  ( 0.1303874742813643239, 0.9914631140645255858, 0.000000000000000000 ) ) ;
#1319 = CARTESIAN_POINT ( 'NONE',  ( 207.8429183184021269, 119.9981648402868331, -50.00000000000000000 ) ) ;
#1320 = CARTESIAN_POINT ( 'NONE',  ( -207.8429183184027238, 119.9981648402860230, 14.70000000000000462 ) ) ;
#1321 = PRODUCT_DEFINITION_SHAPE ( 'NONE', 'NONE',  #7764 ) ;
#1322 = SURFACE_STYLE_FILL_AREA ( #1888 ) ;
#1323 = DIRECTION ( 'NONE',  ( 1.000000000000000000, 0.000000000000000000, 0.000000000000000000 ) ) ;
#1324 = DIRECTION ( 'NONE',  ( 0.000000000000000000, 0.000000000000000000, -1.000000000000000000 ) ) ;
#1325 = VERTEX_POINT ( 'NONE', #3442 ) ;
#1326 = ADVANCED_FACE ( 'NONE', ( #1711 ), #992, .F. ) ;
#1327 = ORIENTED_EDGE ( 'NONE', *, *, #3741, .T. ) ;
#1328 = ORIENTED_EDGE ( 'NONE', *, *, #2081, .F. ) ;
#1329 = TOROIDAL_SURFACE ( 'NONE', #5369, 30.30000000000000071, 0.3000000000000003775 ) ;
#1330 = DIRECTION ( 'NONE',  ( -1.000000000000000000, 0.000000000000000000, 0.000000000000000000 ) ) ;
#1331 = DIRECTION ( 'NONE',  ( 3.081487911019577365E-33, -2.775557561562891967E-17, -1.000000000000000000 ) ) ;
#1332 = CYLINDRICAL_SURFACE ( 'NONE', #6222, 28.50000000000000711 ) ;
#1333 = ADVANCED_FACE ( 'NONE', ( #3407 ), #2862, .F. ) ;
#1334 = ORIENTED_EDGE ( 'NONE', *, *, #7076, .F. ) ;
#1335 = VERTEX_POINT ( 'NONE', #6368 ) ;
#1336 = AXIS2_PLACEMENT_3D ( 'NONE', #5762, #5167, #4621 ) ;
#1337 = VERTEX_POINT ( 'NONE', #5175 ) ;
#1338 = CARTESIAN_POINT ( 'NONE',  ( -68.76644452187068168, 49.96174644486002592, -40.00000000000000000 ) ) ;
#1339 = EDGE_CURVE ( 'NONE', #6807, #5511, #5809, .T. ) ;
#1340 = AXIS2_PLACEMENT_3D ( 'NONE', #5296, #3370, #2237 ) ;
#1341 = LINE ( 'NONE', #675, #2511 ) ;
#1342 = CARTESIAN_POINT ( 'NONE',  ( 8.000000000000000000, 0.000000000000000000, -4.700000000000000178 ) ) ;
#1343 = ORIENTED_EDGE ( 'NONE', *, *, #508, .F. ) ;
#1344 = EDGE_CURVE ( 'NONE', #3392, #7619, #6265, .T. ) ;
#1345 = CIRCLE ( 'NONE', #2867, 5.249999999999991118 ) ;
#1346 = ORIENTED_EDGE ( 'NONE', *, *, #4608, .F. ) ;
#1347 = DIRECTION ( 'NONE',  ( 5.551115123125782702E-17, -0.000000000000000000, 1.000000000000000000 ) ) ;
#1348 = CARTESIAN_POINT ( 'NONE',  ( 0.000000000000000000, 0.000000000000000000, -90.00000000000000000 ) ) ;
#1349 = DIRECTION ( 'NONE',  ( 1.000000000000000000, 0.000000000000000000, 0.000000000000000000 ) ) ;
#1350 = ITEM_DEFINED_TRANSFORMATION ( 'NONE', 'NONE', #666,  #7485 ) ;
#1351 = AXIS2_PLACEMENT_3D ( 'NONE', #6056, #3682, #6766 ) ;
#1352 = DIRECTION ( 'NONE',  ( 1.000000000000000000, 0.000000000000000000, 0.000000000000000000 ) ) ;
#1353 = ORIENTED_EDGE ( 'NONE', *, *, #7213, .T. ) ;
#1354 = DIRECTION ( 'NONE',  ( 1.000000000000000000, 0.000000000000000000, 0.000000000000000000 ) ) ;
#1355 = CONICAL_SURFACE ( 'NONE', #2879, 8.000000000000000000, 1.047197551196596299 ) ;
#1356 = DIRECTION ( 'NONE',  ( -0.000000000000000000, -0.000000000000000000, -1.000000000000000000 ) ) ;
#1357 = DIRECTION ( 'NONE',  ( -0.000000000000000000, -0.000000000000000000, 1.000000000000000000 ) ) ;
#1358 = CARTESIAN_POINT ( 'NONE',  ( -125.2481648402875578, 207.8429183184017859, -50.00000000000000000 ) ) ;
#1359 = APPLICATION_PROTOCOL_DEFINITION ( 'draft international standard', 'automotive_design', 1998, #2040 ) ;
#1360 = CARTESIAN_POINT ( 'NONE',  ( -2.081668171172168513E-14, -9.237604307034017026, -3.985468820183668104 ) ) ;
#1361 = CARTESIAN_POINT ( 'NONE',  ( 0.000000000000000000, 0.000000000000000000, -60.00000000000000711 ) ) ;
#1362 = ORIENTED_EDGE ( 'NONE', *, *, #1084, .F. ) ;
#1363 = EDGE_LOOP ( 'NONE', ( #383, #2492 ) ) ;
#1364 = AXIS2_PLACEMENT_3D ( 'NONE', #4356, #3812, #6774 ) ;
#1365 = EDGE_LOOP ( 'NONE', ( #3798, #3024, #2338 ) ) ;
#1366 = DIRECTION ( 'NONE',  ( -0.000000000000000000, 0.000000000000000000, -1.000000000000000000 ) ) ;
#1367 = CARTESIAN_POINT ( 'NONE',  ( 6.686525924292793022, -5.377136764700165550, -4.383279549040157264 ) ) ;
#1368 = CARTESIAN_POINT ( 'NONE',  ( 5.870234470492294880E-31, -4.203179568131150526E-15, -122.9999999999999716 ) ) ;
#1369 = VECTOR ( 'NONE', #2478, 1000.000000000000000 ) ;
#1370 = ORIENTED_EDGE ( 'NONE', *, *, #2358, .F. ) ;
#1371 = ORIENTED_EDGE ( 'NONE', *, *, #1525, .F. ) ;
#1372 = EDGE_CURVE ( 'NONE', #6339, #1121, #4871, .T. ) ;
#1373 = VERTEX_POINT ( 'NONE', #5397 ) ;
#1374 = UNCERTAINTY_MEASURE_WITH_UNIT (LENGTH_MEASURE( 1.000000000000000082E-05 ), #4771, 'distance_accuracy_value', 'NONE');
#1375 = EDGE_CURVE ( 'NONE', #5121, #6571, #7635, .T. ) ;
#1376 = AXIS2_PLACEMENT_3D ( 'NONE', #772, #4952, #1400 ) ;
#1377 = EDGE_CURVE ( 'NONE', #1051, #6864, #5904, .T. ) ;
#1378 = CARTESIAN_POINT ( 'NONE',  ( 1.499999999999999334, -33.63777638310832430, -3.000000000000000000 ) ) ;
#1379 =( NAMED_UNIT ( * ) PLANE_ANGLE_UNIT ( ) SI_UNIT ( $, .RADIAN. ) );
#1380 = EDGE_CURVE ( 'NONE', #1191, #2413, #1086, .T. ) ;
#1381 = DIRECTION ( 'NONE',  ( -1.000000000000000000, 0.000000000000000000, 0.000000000000000000 ) ) ;
#1382 = CARTESIAN_POINT ( 'NONE',  ( 3.911624228440929052, 29.74389342193576624, 13.00000000000001066 ) ) ;
#1383 = ORIENTED_EDGE ( 'NONE', *, *, #3503, .F. ) ;
#1384 =( GEOMETRIC_REPRESENTATION_CONTEXT ( 3 ) GLOBAL_UNCERTAINTY_ASSIGNED_CONTEXT ( ( #4236 ) ) GLOBAL_UNIT_ASSIGNED_CONTEXT ( ( #6039, #36, #3783 ) ) REPRESENTATION_CONTEXT ( 'NONE', 'WORKASPACE' ) );
#1385 = ADVANCED_FACE ( 'NONE', ( #2250 ), #7086, .F. ) ;
#1386 = ADVANCED_FACE ( 'NONE', ( #7713 ), #4719, .T. ) ;
#1387 = PRODUCT_DEFINITION_SHAPE ( 'NONE', 'NONE',  #6478 ) ;
#1388 = CARTESIAN_POINT ( 'NONE',  ( -4.000000000000004441, 6.928203230275506108, 0.000000000000000000 ) ) ;
#1389 = CARTESIAN_POINT ( 'NONE',  ( 37.49999999999997868, 0.000000000000000000, -82.99999999999998579 ) ) ;
#1390 = VECTOR ( 'NONE', #555, 1000.000000000000000 ) ;
#1391 = CARTESIAN_POINT ( 'NONE',  ( 125.2481648402866199, 207.8429183184022122, -50.00000000000000000 ) ) ;
#1392 = LINE ( 'NONE', #205, #6581 ) ;
#1393 = ORIENTED_EDGE ( 'NONE', *, *, #6504, .T. ) ;
#1394 = CARTESIAN_POINT ( 'NONE',  ( 0.000000000000000000, 0.000000000000000000, -109.9956969048621716 ) ) ;
#1395 = CONICAL_SURFACE ( 'NONE', #2425, 8.000000000000000000, 1.047197551196596299 ) ;
#1396 = CARTESIAN_POINT ( 'NONE',  ( -78.76644452187068168, 49.96174644486002592, -40.00000000000000000 ) ) ;
#1397 = DIRECTION ( 'NONE',  ( 0.000000000000000000, 0.000000000000000000, 1.000000000000000000 ) ) ;
#1398 = DIRECTION ( 'NONE',  ( 1.000000000000000000, 0.000000000000000000, 0.000000000000000000 ) ) ;
#1399 = CARTESIAN_POINT ( 'NONE',  ( -3.499999999999996003, 4.574055794815363937E-15, 37.19999999999999574 ) ) ;
#1400 = DIRECTION ( 'NONE',  ( 1.000000000000000000, 0.000000000000000000, 0.000000000000000000 ) ) ;
#1401 = VERTEX_POINT ( 'NONE', #4164 ) ;
#1402 = ORIENTED_EDGE ( 'NONE', *, *, #1747, .F. ) ;
#1403 = ORIENTED_EDGE ( 'NONE', *, *, #2848, .T. ) ;
#1404 = ORIENTED_EDGE ( 'NONE', *, *, #5880, .F. ) ;
#1405 = CARTESIAN_POINT ( 'NONE',  ( -5.857142857142855874, 7.172931252148781134E-16, 9.480888224575629408 ) ) ;
#1406 = SURFACE_SIDE_STYLE ('',( #819 ) ) ;
#1407 = DIRECTION ( 'NONE',  ( 0.000000000000000000, 0.000000000000000000, 1.000000000000000000 ) ) ;
#1408 = AXIS2_PLACEMENT_3D ( 'NONE', #7465, #6806, #4429 ) ;
#1409 = EDGE_LOOP ( 'NONE', ( #1796, #3155, #6670, #4098, #6477, #628 ) ) ;
#1410 = ORIENTED_EDGE ( 'NONE', *, *, #6203, .T. ) ;
#1411 = AXIS2_PLACEMENT_3D ( 'NONE', #86, #7191, #2390 ) ;
#1412 = DIRECTION ( 'NONE',  ( 0.000000000000000000, 0.000000000000000000, 1.000000000000000000 ) ) ;
#1413 = DIRECTION ( 'NONE',  ( 0.9845265360683707057, 0.1752355551171480841, 0.000000000000000000 ) ) ;
#1414 =( NAMED_UNIT ( * ) PLANE_ANGLE_UNIT ( ) SI_UNIT ( $, .RADIAN. ) );
#1415 = DIRECTION ( 'NONE',  ( 0.1948910352220799835, -0.9808248999643441879, -1.110223024625155986E-18 ) ) ;
#1416 = DIRECTION ( 'NONE',  ( 0.000000000000000000, 0.000000000000000000, -1.000000000000000000 ) ) ;
#1417 = AXIS2_PLACEMENT_3D ( 'NONE', #4268, #1952, #759 ) ;
#1418 = ORIENTED_EDGE ( 'NONE', *, *, #1826, .T. ) ;
#1419 = ADVANCED_FACE ( 'NONE', ( #6619 ), #3461, .F. ) ;
#1420 =( REPRESENTATION_RELATIONSHIP ('NONE','NONE', #1229, #1433 ) REPRESENTATION_RELATIONSHIP_WITH_TRANSFORMATION ( #2744 )SHAPE_REPRESENTATION_RELATIONSHIP( ) );
#1421 = DIRECTION ( 'NONE',  ( -0.000000000000000000, -0.000000000000000000, 1.000000000000000000 ) ) ;
#1422 = DIRECTION ( 'NONE',  ( -0.000000000000000000, 0.000000000000000000, 1.000000000000000000 ) ) ;
#1423 = VECTOR ( 'NONE', #706, 1000.000000000000000 ) ;
#1424 = DIRECTION ( 'NONE',  ( -1.000000000000000000, 0.000000000000000000, 0.000000000000000000 ) ) ;
#1425 = CONTEXT_DEPENDENT_SHAPE_REPRESENTATION ( #1172, #756 ) ;
#1426 = DIRECTION ( 'NONE',  ( 0.000000000000000000, 0.000000000000000000, 1.000000000000000000 ) ) ;
#1427 = EDGE_CURVE ( 'NONE', #1502, #1238, #1345, .T. ) ;
#1428 = VERTEX_POINT ( 'NONE', #4205 ) ;
#1429 = VECTOR ( 'NONE', #190, 1000.000000000000000 ) ;
#1430 = AXIS2_PLACEMENT_3D ( 'NONE', #4502, #985, #870 ) ;
#1431 = FACE_OUTER_BOUND ( 'NONE', #2465, .T. ) ;
#1432 = DIRECTION ( 'NONE',  ( 0.000000000000000000, -1.000000000000000000, 0.000000000000000000 ) ) ;
#1433 = SHAPE_REPRESENTATION ( 'torque nut 08_iso_ISO 10511-M10-N', ( #7485 ), #309 ) ;
#1434 = FACE_OUTER_BOUND ( 'NONE', #4506, .T. ) ;
#1435 = DIRECTION ( 'NONE',  ( 1.000000000000000000, 0.000000000000000000, 0.000000000000000000 ) ) ;
#1436 =( NAMED_UNIT ( * ) SI_UNIT ( $, .STERADIAN. ) SOLID_ANGLE_UNIT ( ) );
#1437 = AXIS2_PLACEMENT_3D ( 'NONE', #4551, #6220, #1517 ) ;
#1438 = DIRECTION ( 'NONE',  ( 0.000000000000000000, 0.000000000000000000, 1.000000000000000000 ) ) ;
#1439 = CARTESIAN_POINT ( 'NONE',  ( 0.000000000000000000, 0.000000000000000000, -82.99999999999998579 ) ) ;
#1440 = ORIENTED_EDGE ( 'NONE', *, *, #7369, .F. ) ;
#1441 = ORIENTED_EDGE ( 'NONE', *, *, #5678, .F. ) ;
#1442 = ORIENTED_EDGE ( 'NONE', *, *, #5782, .F. ) ;
#1443 = EDGE_CURVE ( 'NONE', #7492, #5665, #1126, .T. ) ;
#1444 = CIRCLE ( 'NONE', #5855, 5.249999999999976907 ) ;
#1445 = PRESENTATION_LAYER_ASSIGNMENT (  '', '', ( #4091 ) ) ;
#1446 = CLOSED_SHELL ( 'NONE', ( #6737, #6352, #1475, #5330, #3466, #2829, #4656, #459, #3800, #2519, #2309, #7588, #4374, #5871, #7324, #3599, #2557, #7263, #7513, #700, #4765, #1030, #2895, #40, #4909, #3685, #2653, #2637, #1589, #5674, #181, #5443, #6790, #5617, #2777, #1044, #5963, #4858, #7757, #1575 ) ) ;
#1447 = ORIENTED_EDGE ( 'NONE', *, *, #4957, .T. ) ;
#1448 = DIRECTION ( 'NONE',  ( -1.000000000000000000, -0.000000000000000000, -0.000000000000000000 ) ) ;
#1449 = CARTESIAN_POINT ( 'NONE',  ( -1.499999999999999334, -33.63777638310832430, 0.000000000000000000 ) ) ;
#1450 = CYLINDRICAL_SURFACE ( 'NONE', #3082, 40.00000000000000711 ) ;
#1451 = AXIS2_PLACEMENT_3D ( 'NONE', #6344, #931, #3539 ) ;
#1452 = CLOSED_SHELL ( 'NONE', ( #6022, #6932, #4288, #1326, #7316, #3316, #3412, #1132, #1867, #4657, #7422, #4128, #2074, #3114, #3945, #5098, #5656, #2984, #6063, #3801, #2170, #3359, #3980, #170, #5923, #3507, #6543, #4032, #6107, #4312, #1724, #2466, #1280 ) ) ;
#1453 = PRODUCT ( 'circlip for shafts heavy_din_Circlip DIN 471 - 60 x 3', 'circlip for shafts heavy_din_Circlip DIN 471 - 60 x 3', '', ( #5587 ) ) ;
#1454 = ORIENTED_EDGE ( 'NONE', *, *, #2012, .T. ) ;
#1455 = ORIENTED_EDGE ( 'NONE', *, *, #4024, .T. ) ;
#1456 = PRODUCT_DEFINITION_CONTEXT ( 'detailed design', #817, 'design' ) ;
#1457 = DIRECTION ( 'NONE',  ( 1.000000000000000000, 0.000000000000000000, 0.000000000000000000 ) ) ;
#1458 = FILL_AREA_STYLE_COLOUR ( '', #7110 ) ;
#1459 = CARTESIAN_POINT ( 'NONE',  ( 0.000000000000000000, 0.000000000000000000, -4.700000000000000178 ) ) ;
#1460 = LINE ( 'NONE', #3759, #6409 ) ;
#1461 = AXIS2_PLACEMENT_3D ( 'NONE', #5654, #7541, #3255 ) ;
#1462 = CARTESIAN_POINT ( 'NONE',  ( -5.134781488891348999E-13, 239.9963296805737230, -50.00000000000000000 ) ) ;
#1463 = ORIENTED_EDGE ( 'NONE', *, *, #3212, .F. ) ;
#1464 = ADVANCED_FACE ( 'NONE', ( #5356 ), #7645, .T. ) ;
#1465 = AXIS2_PLACEMENT_3D ( 'NONE', #1909, #5531, #2395 ) ;
#1466 = CARTESIAN_POINT ( 'NONE',  ( 129.9038105676649764, 75.00000000000153477, 0.000000000000000000 ) ) ;
#1467 = DIRECTION ( 'NONE',  ( 1.000000000000000000, 0.000000000000000000, 0.000000000000000000 ) ) ;
#1468 = CARTESIAN_POINT ( 'NONE',  ( 5.459126460941067016, -34.89491303563345070, 0.000000000000000000 ) ) ;
#1469 = DIRECTION ( 'NONE',  ( 1.000000000000000000, 0.000000000000000000, 0.000000000000000000 ) ) ;
#1470 = ORIENTED_EDGE ( 'NONE', *, *, #7693, .T. ) ;
#1471 = AXIS2_PLACEMENT_3D ( 'NONE', #5311, #1685, #2953 ) ;
#1472 =( REPRESENTATION_RELATIONSHIP ('NONE','NONE', #1229, #1433 ) REPRESENTATION_RELATIONSHIP_WITH_TRANSFORMATION ( #1200 )SHAPE_REPRESENTATION_RELATIONSHIP( ) );
#1473 = CARTESIAN_POINT ( 'NONE',  ( -73.76644452187068168, 49.96174644486002592, -40.00000000000000000 ) ) ;
#1474 = ADVANCED_FACE ( 'NONE', ( #1733 ), #4045, .F. ) ;
#1475 = ADVANCED_FACE ( 'NONE', ( #3538 ), #538, .T. ) ;
#1476 = CYLINDRICAL_SURFACE ( 'NONE', #2701, 150.0000000000000568 ) ;
#1477 = DIRECTION ( 'NONE',  ( -0.000000000000000000, -0.000000000000000000, -1.000000000000000000 ) ) ;
#1478 = DIRECTION ( 'NONE',  ( -1.000000000000000000, 0.000000000000000000, 0.000000000000000000 ) ) ;
#1479 = APPLICATION_PROTOCOL_DEFINITION ( 'draft international standard', 'automotive_design', 1998, #2795 ) ;
#1480 = EDGE_CURVE ( 'NONE', #4264, #669, #7752, .T. ) ;
#1481 = DIRECTION ( 'NONE',  ( 3.081487911019577365E-33, -2.775557561562891967E-17, -1.000000000000000000 ) ) ;
#1482 = EDGE_LOOP ( 'NONE', ( #6953, #7658, #5675, #1661, #7308, #6188, #4056, #2700 ) ) ;
#1483 = VERTEX_POINT ( 'NONE', #2371 ) ;
#1484 = CIRCLE ( 'NONE', #5392, 150.0000000000000568 ) ;
#1485 = ORIENTED_EDGE ( 'NONE', *, *, #5782, .T. ) ;
#1486 = EDGE_CURVE ( 'NONE', #7492, #2049, #3874, .T. ) ;
#1487 = EDGE_LOOP ( 'NONE', ( #7576, #3858, #7591, #1404 ) ) ;
#1488 = DIRECTION ( 'NONE',  ( 0.8660254037844382635, -0.5000000000000005551, 0.000000000000000000 ) ) ;
#1489 = FACE_OUTER_BOUND ( 'NONE', #2089, .T. ) ;
#1490 = CIRCLE ( 'NONE', #6533, 5.249999999999976907 ) ;
#1491 = DIRECTION ( 'NONE',  ( 1.000000000000000000, 0.000000000000000000, 0.000000000000000000 ) ) ;
#1492 = ADVANCED_FACE ( 'NONE', ( #5234, #1165 ), #581, .T. ) ;
#1493 = ORIENTED_EDGE ( 'NONE', *, *, #5383, .F. ) ;
#1494 = AXIS2_PLACEMENT_3D ( 'NONE', #7712, #1046, #2332 ) ;
#1495 = ORIENTED_EDGE ( 'NONE', *, *, #7454, .F. ) ;
#1496 = VERTEX_POINT ( 'NONE', #3106 ) ;
#1497 = DIRECTION ( 'NONE',  ( 0.000000000000000000, 0.000000000000000000, 1.000000000000000000 ) ) ;
#1498 = SURFACE_STYLE_FILL_AREA ( #828 ) ;
#1499 = AXIS2_PLACEMENT_3D ( 'NONE', #487, #5814, #4631 ) ;
#1500 = FACE_OUTER_BOUND ( 'NONE', #7185, .T. ) ;
#1501 = DIRECTION ( 'NONE',  ( -0.000000000000000000, -0.000000000000000000, 1.000000000000000000 ) ) ;
#1502 = VERTEX_POINT ( 'NONE', #1358 ) ;
#1503 = AXIS2_PLACEMENT_3D ( 'NONE', #3151, #4398, #5627 ) ;
#1504 = CARTESIAN_POINT ( 'NONE',  ( -28.32536770618215982, 3.150165759062969695, 10.00000000000000000 ) ) ;
#1505 = CARTESIAN_POINT ( 'NONE',  ( 28.32536770618215982, -3.150165759062971471, 13.00000000000000178 ) ) ;
#1506 = CARTESIAN_POINT ( 'NONE',  ( -0.6543471694412569262, -8.859816792613647962, -4.203584543331202461 ) ) ;
#1507 = AXIS2_PLACEMENT_3D ( 'NONE', #6309, #7594, #7009 ) ;
#1508 = CARTESIAN_POINT ( 'NONE',  ( 145.1064334105730893, 38.00161816111175739, 10.00000000000000000 ) ) ;
#1509 = EDGE_LOOP ( 'NONE', ( #3965, #7043, #5591, #1455 ) ) ;
#1510 = CARTESIAN_POINT ( 'NONE',  ( -68.76644452187068168, 49.96174644486002592, 25.00000000000000000 ) ) ;
#1511 = AXIS2_PLACEMENT_3D ( 'NONE', #5290, #6517, #6472 ) ;
#1512 = DIRECTION ( 'NONE',  ( -0.000000000000000000, -0.000000000000000000, 1.000000000000000000 ) ) ;
#1513 = FACE_BOUND ( 'NONE', #7758, .T. ) ;
#1514 = CARTESIAN_POINT ( 'NONE',  ( -10.00000000000000000, 42.00000000000000000, 0.000000000000000000 ) ) ;
#1515 = CARTESIAN_POINT ( 'NONE',  ( 37.49999999999997868, 0.000000000000000000, -90.00000000000000000 ) ) ;
#1516 = CONTEXT_DEPENDENT_SHAPE_REPRESENTATION ( #2690, #193 ) ;
#1517 = DIRECTION ( 'NONE',  ( 1.000000000000000000, 0.000000000000000000, 0.000000000000000000 ) ) ;
#1518 = ADVANCED_FACE ( 'NONE', ( #6141 ), #730, .F. ) ;
#1519 = VECTOR ( 'NONE', #1931, 1000.000000000000000 ) ;
#1520 = ORIENTED_EDGE ( 'NONE', *, *, #4655, .T. ) ;
#1521 = ORIENTED_EDGE ( 'NONE', *, *, #7357, .F. ) ;
#1522 = EDGE_CURVE ( 'NONE', #2129, #7160, #1282, .T. ) ;
#1523 = ADVANCED_FACE ( 'NONE', ( #7396 ), #3655, .F. ) ;
#1524 = ORIENTED_EDGE ( 'NONE', *, *, #2927, .F. ) ;
#1525 = EDGE_CURVE ( 'NONE', #4724, #194, #4873, .T. ) ;
#1526 = VERTEX_POINT ( 'NONE', #7284 ) ;
#1527 = FACE_OUTER_BOUND ( 'NONE', #6010, .T. ) ;
#1528 = DIRECTION ( 'NONE',  ( -1.000000000000000000, 0.000000000000000000, 0.000000000000000000 ) ) ;
#1529 =( NAMED_UNIT ( * ) PLANE_ANGLE_UNIT ( ) SI_UNIT ( $, .RADIAN. ) );
#1530 = FACE_OUTER_BOUND ( 'NONE', #2638, .T. ) ;
#1531 = EDGE_CURVE ( 'NONE', #1219, #5930, #7143, .T. ) ;
#1532 = VERTEX_POINT ( 'NONE', #5543 ) ;
#1533 = EDGE_LOOP ( 'NONE', ( #6280, #3924 ) ) ;
#1534 = ORIENTED_EDGE ( 'NONE', *, *, #4067, .T. ) ;
#1535 = CARTESIAN_POINT ( 'NONE',  ( -68.76644452187068168, 49.96174644486002592, 25.00000000000000000 ) ) ;
#1536 = SHAPE_REPRESENTATION_RELATIONSHIP ( 'NONE' , 'NONE' ,  #5768, #1719 ) ;
#1537 = VECTOR ( 'NONE', #1237, 1000.000000000000000 ) ;
#1538 = DIRECTION ( 'NONE',  ( -0.000000000000000000, -0.000000000000000000, -1.000000000000000000 ) ) ;
#1539 = DIRECTION ( 'NONE',  ( 1.000000000000000000, 2.398081733190338127E-14, 0.000000000000000000 ) ) ;
#1540 = VERTEX_POINT ( 'NONE', #2563 ) ;
#1541 = AXIS2_PLACEMENT_3D ( 'NONE', #3396, #7060, #944 ) ;
#1542 = DIRECTION ( 'NONE',  ( -0.07885359840235164897, 0.9968862071565643967, 0.000000000000000000 ) ) ;
#1543 = DIRECTION ( 'NONE',  ( -0.000000000000000000, -0.000000000000000000, 1.000000000000000000 ) ) ;
#1544 = DIRECTION ( 'NONE',  ( -0.000000000000000000, -0.000000000000000000, 1.000000000000000000 ) ) ;
#1545 = DIRECTION ( 'NONE',  ( 1.000000000000000000, 0.000000000000000000, 0.000000000000000000 ) ) ;
#1546 = TOROIDAL_SURFACE ( 'NONE', #5699, 6.713333333332999864, 1.286666666666999914 ) ;
#1547 = CYLINDRICAL_SURFACE ( 'NONE', #6081, 5.249999999999976907 ) ;
#1548 = ORIENTED_EDGE ( 'NONE', *, *, #7688, .F. ) ;
#1549 = DIRECTION ( 'NONE',  ( 1.000000000000000000, 0.000000000000000000, 0.000000000000000000 ) ) ;
#1550 = CONICAL_SURFACE ( 'NONE', #3824, 5.000000000000000888, 0.9599310885968824758 ) ;
#1551 = LINE ( 'NONE', #5140, #1712 ) ;
#1552 = CARTESIAN_POINT ( 'NONE',  ( -4.665299213380359689, 29.63502966507089909, -79.99999999999995737 ) ) ;
#1553 = PLANE ( 'NONE',  #489 ) ;
#1554 = DIRECTION ( 'NONE',  ( 1.000000000000000000, 0.000000000000000000, 0.000000000000000000 ) ) ;
#1555 = CONTEXT_DEPENDENT_SHAPE_REPRESENTATION ( #2296, #3855 ) ;
#1556 = DIRECTION ( 'NONE',  ( 1.000000000000000000, 0.000000000000000000, 0.000000000000000000 ) ) ;
#1557 = CIRCLE ( 'NONE', #550, 4.999999999999990230 ) ;
#1558 = ORIENTED_EDGE ( 'NONE', *, *, #3708, .T. ) ;
#1559 = VECTOR ( 'NONE', #6445, 1000.000000000000000 ) ;
#1560 = ORIENTED_EDGE ( 'NONE', *, *, #7226, .F. ) ;
#1561 = VERTEX_POINT ( 'NONE', #4319 ) ;
#1562 = DIRECTION ( 'NONE',  ( -5.551115123125782702E-17, 0.000000000000000000, -1.000000000000000000 ) ) ;
#1563 = CARTESIAN_POINT ( 'NONE',  ( 199.9963296805737230, -4.796075449120964792E-12, 576.0908266162076643 ) ) ;
#1564 = COLOUR_RGB ( '',0.8941176470588234615, 0.8941176470588234615, 0.8941176470588234615 ) ;
#1565 = CARTESIAN_POINT ( 'NONE',  ( 8.000000000000000000, -4.618802153517011178, -0.7145311798163319628 ) ) ;
#1566 = CARTESIAN_POINT ( 'NONE',  ( -8.000000000000000000, 4.618802153517003184, -0.7145311798163286321 ) ) ;
#1567 = CARTESIAN_POINT ( 'NONE',  ( -68.76644452187068168, 49.96174644486002592, 14.69999999999999929 ) ) ;
#1568 = DIRECTION ( 'NONE',  ( 0.000000000000000000, 0.000000000000000000, 1.000000000000000000 ) ) ;
#1569 = EDGE_CURVE ( 'NONE', #5426, #1540, #718, .T. ) ;
#1570 = AXIS2_PLACEMENT_3D ( 'NONE', #3623, #6029, #621 ) ;
#1571 = ORIENTED_EDGE ( 'NONE', *, *, #5379, .F. ) ;
#1572 = VERTEX_POINT ( 'NONE', #653 ) ;
#1573 = VERTEX_POINT ( 'NONE', #4989 ) ;
#1574 = DIRECTION ( 'NONE',  ( -0.000000000000000000, -0.000000000000000000, 1.000000000000000000 ) ) ;
#1575 = ADVANCED_FACE ( 'NONE', ( #4243 ), #3067, .T. ) ;
#1576 = APPLICATION_PROTOCOL_DEFINITION ( 'draft international standard', 'automotive_design', 1998, #405 ) ;
#1577 = STYLED_ITEM ( 'NONE', ( #3746 ), #7262 ) ;
#1578 = CARTESIAN_POINT ( 'NONE',  ( 0.000000000000000000, 0.000000000000000000, 0.000000000000000000 ) ) ;
#1579 =( REPRESENTATION_RELATIONSHIP ('NONE','NONE', #1229, #1433 ) REPRESENTATION_RELATIONSHIP_WITH_TRANSFORMATION ( #4157 )SHAPE_REPRESENTATION_RELATIONSHIP( ) );
#1580 = EDGE_CURVE ( 'NONE', #2827, #7413, #3032, .T. ) ;
#1581 = DIRECTION ( 'NONE',  ( 1.000000000000000000, 0.000000000000000000, 0.000000000000000000 ) ) ;
#1582 = VERTEX_POINT ( 'NONE', #3732 ) ;
#1583 = EDGE_CURVE ( 'NONE', #5377, #1095, #3495, .T. ) ;
#1584 = DIRECTION ( 'NONE',  ( -0.000000000000000000, -0.000000000000000000, 1.000000000000000000 ) ) ;
#1585 = LINE ( 'NONE', #3876, #6474 ) ;
#1586 = CIRCLE ( 'NONE', #198, 5.249999999999976907 ) ;
#1587 = CARTESIAN_POINT ( 'NONE',  ( 4.000000000000005329, -6.928203230275506108, 0.000000000000000000 ) ) ;
#1588 = LINE ( 'NONE', #5293, #531 ) ;
#1589 = ADVANCED_FACE ( 'NONE', ( #4357 ), #3691, .F. ) ;
#1590 = ORIENTED_EDGE ( 'NONE', *, *, #5900, .F. ) ;
#1591 = AXIS2_PLACEMENT_3D ( 'NONE', #7063, #5328, #7728 ) ;
#1592 = DIRECTION ( 'NONE',  ( 1.000000000000000000, 0.000000000000000000, 0.000000000000000000 ) ) ;
#1593 =( NAMED_UNIT ( * ) SI_UNIT ( $, .STERADIAN. ) SOLID_ANGLE_UNIT ( ) );
#1594 = CARTESIAN_POINT ( 'NONE',  ( 0.000000000000000000, 0.000000000000000000, 0.000000000000000000 ) ) ;
#1595 = CARTESIAN_POINT ( 'NONE',  ( 2.750000000000000000, -33.63777638310832430, -3.000000000000000000 ) ) ;
#1596 = CARTESIAN_POINT ( 'NONE',  ( 29.99999999999999289, 0.000000000000000000, -139.9999999999999716 ) ) ;
#1597 = TOROIDAL_SURFACE ( 'NONE', #2369, 37.19999999999999574, 0.3000000000000007661 ) ;
#1598 = LINE ( 'NONE', #3376, #1959 ) ;
#1599 = ORIENTED_EDGE ( 'NONE', *, *, #1339, .T. ) ;
#1600 = ORIENTED_EDGE ( 'NONE', *, *, #6442, .F. ) ;
#1601 = VERTEX_POINT ( 'NONE', #2597 ) ;
#1602 = AXIS2_PLACEMENT_3D ( 'NONE', #4476, #7433, #1435 ) ;
#1603 = DIRECTION ( 'NONE',  ( -0.000000000000000000, -0.000000000000000000, 1.000000000000000000 ) ) ;
#1604 = CYLINDRICAL_SURFACE ( 'NONE', #4640, 5.857142857142855874 ) ;
#1605 = DIRECTION ( 'NONE',  ( 1.000000000000000000, 0.000000000000000000, 0.000000000000000000 ) ) ;
#1606 = FACE_OUTER_BOUND ( 'NONE', #1487, .T. ) ;
#1607 = AXIS2_PLACEMENT_3D ( 'NONE', #1912, #4863, #169 ) ;
#1608 = B_SPLINE_CURVE_WITH_KNOTS ( 'NONE', 3,
 ( #375, #1771, #4005, #2991, #5824, #1085, #4162, #4639 ),
 .UNSPECIFIED., .F., .F.,
 ( 4, 2, 2, 4 ),
 ( 0.004673709593152164388, 0.005837709341827650340, 0.007001709090503136293, 0.009329708587854108198 ),
 .UNSPECIFIED. ) ;
#1609 = VERTEX_POINT ( 'NONE', #5430 ) ;
#1610 = VERTEX_POINT ( 'NONE', #6099 ) ;
#1611 = VERTEX_POINT ( 'NONE', #63 ) ;
#1612 = AXIS2_PLACEMENT_3D ( 'NONE', #11, #5374, #1188 ) ;
#1613 = DIRECTION ( 'NONE',  ( -1.000000000000000000, -0.000000000000000000, -0.000000000000000000 ) ) ;
#1614 = LINE ( 'NONE', #2260, #7101 ) ;
#1615 = VECTOR ( 'NONE', #25, 1000.000000000000000 ) ;
#1616 = DIRECTION ( 'NONE',  ( 0.000000000000000000, 0.000000000000000000, 1.000000000000000000 ) ) ;
#1617 = ADVANCED_FACE ( 'NONE', ( #4396 ), #3187, .F. ) ;
#1618 = EDGE_LOOP ( 'NONE', ( #1560, #2255, #813, #2345 ) ) ;
#1619 = EDGE_CURVE ( 'NONE', #3881, #2383, #178, .T. ) ;
#1620 = ADVANCED_FACE ( 'NONE', ( #6812 ), #2247, .F. ) ;
#1621 = EDGE_CURVE ( 'NONE', #3939, #3350, #6218, .T. ) ;
#1622 = DIRECTION ( 'NONE',  ( 0.000000000000000000, 0.000000000000000000, -1.000000000000000000 ) ) ;
#1623 = CARTESIAN_POINT ( 'NONE',  ( -73.76644452187072432, 49.96174644486006855, -40.00000000000000000 ) ) ;
#1624 = APPLICATION_CONTEXT ( 'automotive_design' ) ;
#1625 = DIRECTION ( 'NONE',  ( -1.000000000000000000, 0.000000000000000000, 0.000000000000000000 ) ) ;
#1626 = DIRECTION ( 'NONE',  ( 1.000000000000000000, 0.000000000000000000, 0.000000000000000000 ) ) ;
#1627 = ORIENTED_EDGE ( 'NONE', *, *, #5133, .F. ) ;
#1628 = VECTOR ( 'NONE', #4680, 1000.000000000000000 ) ;
#1629 = EDGE_CURVE ( 'NONE', #6375, #3955, #7547, .T. ) ;
#1630 = EDGE_LOOP ( 'NONE', ( #5952, #7300, #6677, #6036 ) ) ;
#1631 = FACE_OUTER_BOUND ( 'NONE', #3790, .T. ) ;
#1632 = SURFACE_STYLE_USAGE ( .BOTH. , #7073 ) ;
#1633 = CIRCLE ( 'NONE', #5418, 5.000000000000004441 ) ;
#1634 = DIRECTION ( 'NONE',  ( 0.000000000000000000, 0.000000000000000000, -1.000000000000000000 ) ) ;
#1635 = FACE_OUTER_BOUND ( 'NONE', #3761, .T. ) ;
#1636 = CARTESIAN_POINT ( 'NONE',  ( 0.000000000000000000, 0.000000000000000000, -4.700000000000000178 ) ) ;
#1637 = CONTEXT_DEPENDENT_SHAPE_REPRESENTATION ( #6421, #2535 ) ;
#1638 = CARTESIAN_POINT ( 'NONE',  ( 0.000000000000000000, 0.000000000000000000, 9.480888224575629408 ) ) ;
#1639 = ORIENTED_EDGE ( 'NONE', *, *, #6385, .F. ) ;
#1640 = ORIENTED_EDGE ( 'NONE', *, *, #6203, .F. ) ;
#1641 = AXIS2_PLACEMENT_3D ( 'NONE', #3794, #6045, #3674 ) ;
#1642 = VERTEX_POINT ( 'NONE', #3296 ) ;
#1643 = DIRECTION ( 'NONE',  ( 0.000000000000000000, 0.000000000000000000, -1.000000000000000000 ) ) ;
#1644 = CARTESIAN_POINT ( 'NONE',  ( 0.000000000000000000, 0.000000000000000000, 9.480888224575629408 ) ) ;
#1645 = CARTESIAN_POINT ( 'NONE',  ( 0.000000000000000000, 0.000000000000000000, 0.000000000000000000 ) ) ;
#1646 = DIRECTION ( 'NONE',  ( 1.000000000000000000, 0.000000000000000000, 0.000000000000000000 ) ) ;
#1647 = CONICAL_SURFACE ( 'NONE', #4166, 4.999999999999990230, 0.7853981633974482790 ) ;
#1648 = CYLINDRICAL_SURFACE ( 'NONE', #4078, 150.0000000000000568 ) ;
#1649 = CARTESIAN_POINT ( 'NONE',  ( -119.9981648402875578, 207.8429183184017859, -120.0000000000000000 ) ) ;
#1650 = EDGE_LOOP ( 'NONE', ( #6505, #6800, #3164, #3817 ) ) ;
#1651 = VERTEX_POINT ( 'NONE', #5029 ) ;
#1652 = AXIS2_PLACEMENT_3D ( 'NONE', #3931, #2716, #7556 ) ;
#1653 = EDGE_LOOP ( 'NONE', ( #4040, #404, #1082, #1782 ) ) ;
#1654 = AXIS2_PLACEMENT_3D ( 'NONE', #1124, #2331, #5941 ) ;
#1655 = CARTESIAN_POINT ( 'NONE',  ( -1.728922298134113098E-15, 8.513302795252935035E-16, 13.00000000000000178 ) ) ;
#1656 = CARTESIAN_POINT ( 'NONE',  ( 26.26644452187053957, 80.83980388508807380, 0.000000000000000000 ) ) ;
#1657 = FILL_AREA_STYLE_COLOUR ( '', #1564 ) ;
#1658 = FACE_OUTER_BOUND ( 'NONE', #6506, .T. ) ;
#1659 = CARTESIAN_POINT ( 'NONE',  ( -0.5700000000000001732, -28.49429942988597020, 0.000000000000000000 ) ) ;
#1660 = ORIENTED_EDGE ( 'NONE', *, *, #5572, .T. ) ;
#1661 = ORIENTED_EDGE ( 'NONE', *, *, #5964, .T. ) ;
#1662 = DIRECTION ( 'NONE',  ( 0.4999999999999979461, 0.8660254037844398178, 0.000000000000000000 ) ) ;
#1663 = CARTESIAN_POINT ( 'NONE',  ( 129.9038105676649764, 75.00000000000153477, 10.00000000000000000 ) ) ;
#1664 = CARTESIAN_POINT ( 'NONE',  ( 0.000000000000000000, 0.000000000000000000, 0.000000000000000000 ) ) ;
#1665 = CARTESIAN_POINT ( 'NONE',  ( -20.63749999999999929, 0.000000000000000000, 0.000000000000000000 ) ) ;
#1666 = AXIS2_PLACEMENT_3D ( 'NONE', #2734, #5765, #3954 ) ;
#1667 = ORIENTED_EDGE ( 'NONE', *, *, #1731, .F. ) ;
#1668 = EDGE_CURVE ( 'NONE', #2714, #2100, #3369, .T. ) ;
#1669 = ORIENTED_EDGE ( 'NONE', *, *, #4327, .F. ) ;
#1670 = CARTESIAN_POINT ( 'NONE',  ( -7.347286611336973472, -4.995646404165286825, -0.4969600502617561033 ) ) ;
#1671 = CARTESIAN_POINT ( 'NONE',  ( -207.8429183184020985, 119.9981648402869467, -8.673617379884035472E-15 ) ) ;
#1672 = CIRCLE ( 'NONE', #5195, 29.99999999999999289 ) ;
#1673 =( LENGTH_UNIT ( ) NAMED_UNIT ( * ) SI_UNIT ( .MILLI., .METRE. ) );
#1674 = PRODUCT_DEFINITION_FORMATION_WITH_SPECIFIED_SOURCE ( 'ANY', '', #3788, .NOT_KNOWN. ) ;
#1675 = CARTESIAN_POINT ( 'NONE',  ( 2.583028308771596837, 28.38270538120150377, 13.00000000000000178 ) ) ;
#1676 = CARTESIAN_POINT ( 'NONE',  ( 0.000000000000000000, 0.000000000000000000, -3.000000000000000000 ) ) ;
#1677 = EDGE_CURVE ( 'NONE', #5637, #7551, #3223, .T. ) ;
#1678 = DIRECTION ( 'NONE',  ( 0.000000000000000000, 0.000000000000000000, 1.000000000000000000 ) ) ;
#1679 = ORIENTED_EDGE ( 'NONE', *, *, #2459, .F. ) ;
#1680 = ORIENTED_EDGE ( 'NONE', *, *, #7692, .F. ) ;
#1681 = VECTOR ( 'NONE', #4745, 1000.000000000000000 ) ;
#1682 = EDGE_LOOP ( 'NONE', ( #5830, #1092, #2508, #3562 ) ) ;
#1683 = DIRECTION ( 'NONE',  ( -1.000000000000000000, 0.000000000000000000, 0.000000000000000000 ) ) ;
#1684 = LINE ( 'NONE', #4676, #5524 ) ;
#1685 = DIRECTION ( 'NONE',  ( -0.000000000000000000, -0.000000000000000000, 1.000000000000000000 ) ) ;
#1686 = DIRECTION ( 'NONE',  ( 0.3090169943749447867, 0.9510565162951546414, 0.000000000000000000 ) ) ;
#1687 = AXIS2_PLACEMENT_3D ( 'NONE', #5556, #1936, #1859 ) ;
#1688 = EDGE_CURVE ( 'NONE', #3738, #1337, #2044, .T. ) ;
#1689 = CARTESIAN_POINT ( 'NONE',  ( 26.82422866010495710, 9.628642520646586433, -119.9999999999999716 ) ) ;
#1690 = FACE_OUTER_BOUND ( 'NONE', #6336, .T. ) ;
#1691 = EDGE_CURVE ( 'NONE', #6167, #587, #1098, .T. ) ;
#1692 = EDGE_LOOP ( 'NONE', ( #3302, #4764, #4390, #7015 ) ) ;
#1693 = EDGE_LOOP ( 'NONE', ( #1306, #6106, #1845, #1679, #5241, #2719 ) ) ;
#1694 = CONICAL_SURFACE ( 'NONE', #5348, 8.000000000000000000, 1.047197551196596299 ) ;
#1695 = AXIS2_PLACEMENT_3D ( 'NONE', #5613, #2620, #202 ) ;
#1696 = EDGE_LOOP ( 'NONE', ( #4031, #1485, #7301, #4838 ) ) ;
#1697 = DIRECTION ( 'NONE',  ( -0.000000000000000000, -0.000000000000000000, -1.000000000000000000 ) ) ;
#1698 = PLANE ( 'NONE',  #2023 ) ;
#1699 = CARTESIAN_POINT ( 'NONE',  ( -68.76644452187068168, 49.96174644486002592, -40.00000000000000000 ) ) ;
#1700 = CONICAL_SURFACE ( 'NONE', #186, 8.000000000000000000, 1.047197551196596299 ) ;
#1701 = DIRECTION ( 'NONE',  ( -0.000000000000000000, 0.000000000000000000, -1.000000000000000000 ) ) ;
#1702 = EDGE_LOOP ( 'NONE', ( #6978, #306, #5696, #595, #4493, #5519 ) ) ;
#1703 = PRESENTATION_LAYER_ASSIGNMENT (  '', '', ( #5856 ) ) ;
#1704 = DIRECTION ( 'NONE',  ( 1.000000000000000000, 0.000000000000000000, 0.000000000000000000 ) ) ;
#1705 = CARTESIAN_POINT ( 'NONE',  ( 213.0929183184020985, 119.9981648402868331, -50.00000000000000000 ) ) ;
#1706 = DIRECTION ( 'NONE',  ( 1.000000000000000000, 0.000000000000000000, 0.000000000000000000 ) ) ;
#1707 = CARTESIAN_POINT ( 'NONE',  ( -4.339467034331194739, -6.732211846623401996, -4.699999999999999289 ) ) ;
#1708 = EDGE_LOOP ( 'NONE', ( #1900, #7024 ) ) ;
#1709 = PRODUCT_RELATED_PRODUCT_CATEGORY ( 'part', '', ( #7248 ) ) ;
#1710 = VERTEX_POINT ( 'NONE', #2668 ) ;
#1711 = FACE_OUTER_BOUND ( 'NONE', #87, .T. ) ;
#1712 = VECTOR ( 'NONE', #6252, 1000.000000000000000 ) ;
#1713 = CYLINDRICAL_SURFACE ( 'NONE', #73, 35.25000000000000000 ) ;
#1714 = DIRECTION ( 'NONE',  ( 1.000000000000000000, 0.000000000000000000, 0.000000000000000000 ) ) ;
#1715 = LINE ( 'NONE', #4705, #5601 ) ;
#1716 = DIRECTION ( 'NONE',  ( 1.000000000000000000, 0.000000000000000000, 0.000000000000000000 ) ) ;
#1717 = DIRECTION ( 'NONE',  ( 1.000000000000000000, 0.000000000000000000, 0.000000000000000000 ) ) ;
#1718 = CONTEXT_DEPENDENT_SHAPE_REPRESENTATION ( #7124, #5545 ) ;
#1719 = ADVANCED_BREP_SHAPE_REPRESENTATION ( '', ( #3160, #7485 ), #7608 ) ;
#1720 = FACE_OUTER_BOUND ( 'NONE', #483, .T. ) ;
#1721 = PRODUCT_DEFINITION_CONTEXT ( 'detailed design', #3243, 'design' ) ;
#1722 = VERTEX_POINT ( 'NONE', #5735 ) ;
#1723 = CIRCLE ( 'NONE', #79, 40.00000000000000000 ) ;
#1724 = ADVANCED_FACE ( 'NONE', ( #3922, #5658 ), #920, .F. ) ;
#1725 = EDGE_LOOP ( 'NONE', ( #3720, #6967 ) ) ;
#1726 = ORIENTED_EDGE ( 'NONE', *, *, #2687, .T. ) ;
#1727 = EDGE_CURVE ( 'NONE', #194, #5633, #2123, .T. ) ;
#1728 = ADVANCED_FACE ( 'NONE', ( #5694 ), #5143, .T. ) ;
#1729 = CARTESIAN_POINT ( 'NONE',  ( -2.309976723937611887, 7.903938623646864059, -4.569346954796190019 ) ) ;
#1730 = VECTOR ( 'NONE', #6808, 1000.000000000000000 ) ;
#1731 = EDGE_CURVE ( 'NONE', #6982, #2714, #5123, .T. ) ;
#1732 = CARTESIAN_POINT ( 'NONE',  ( 8.000000000000000000, -0.7805016046290997878, -3.218725199566340056E-17 ) ) ;
#1733 = FACE_OUTER_BOUND ( 'NONE', #5351, .T. ) ;
#1734 = DIRECTION ( 'NONE',  ( -0.5221611096052830581, -0.8528468652787437598, 0.000000000000000000 ) ) ;
#1735 = FACE_OUTER_BOUND ( 'NONE', #2463, .T. ) ;
#1736 = CARTESIAN_POINT ( 'NONE',  ( 0.000000000000000000, 0.000000000000000000, 10.00000000000000000 ) ) ;
#1737 = ORIENTED_EDGE ( 'NONE', *, *, #2729, .F. ) ;
#1738 = EDGE_CURVE ( 'NONE', #1573, #322, #3257, .T. ) ;
#1739 = AXIS2_PLACEMENT_3D ( 'NONE', #1645, #4123, #2834 ) ;
#1740 = ORIENTED_EDGE ( 'NONE', *, *, #6270, .F. ) ;
#1741 = UNCERTAINTY_MEASURE_WITH_UNIT (LENGTH_MEASURE( 1.000000000000000082E-05 ), #1216, 'distance_accuracy_value', 'NONE');
#1742 = ADVANCED_FACE ( 'NONE', ( #330 ), #6850, .F. ) ;
#1743 =( REPRESENTATION_RELATIONSHIP ('NONE','NONE', #1229, #7725 ) REPRESENTATION_RELATIONSHIP_WITH_TRANSFORMATION ( #1955 )SHAPE_REPRESENTATION_RELATIONSHIP( ) );
#1744 = ORIENTED_EDGE ( 'NONE', *, *, #5346, .T. ) ;
#1745 = DIRECTION ( 'NONE',  ( 0.000000000000000000, 0.000000000000000000, 1.000000000000000000 ) ) ;
#1746 = FACE_BOUND ( 'NONE', #3075, .T. ) ;
#1747 = EDGE_CURVE ( 'NONE', #115, #7619, #5623, .T. ) ;
#1748 = AXIS2_PLACEMENT_3D ( 'NONE', #7742, #5385, #2241 ) ;
#1749 = CARTESIAN_POINT ( 'NONE',  ( -350.0000000000000000, 37.15382499588017140, -82.99999999999998579 ) ) ;
#1750 = ORIENTED_EDGE ( 'NONE', *, *, #6829, .T. ) ;
#1751 = CIRCLE ( 'NONE', #4509, 5.857142857142856762 ) ;
#1752 = DIRECTION ( 'NONE',  ( -0.000000000000000000, -0.000000000000000000, -1.000000000000000000 ) ) ;
#1753 = FACE_OUTER_BOUND ( 'NONE', #2499, .T. ) ;
#1754 = CYLINDRICAL_SURFACE ( 'NONE', #5016, 29.99999999999999289 ) ;
#1755 = AXIS2_PLACEMENT_3D ( 'NONE', #1010, #417, #2837 ) ;
#1756 = CARTESIAN_POINT ( 'NONE',  ( -63.76644452187067458, 49.96174644486002592, -40.00000000000000000 ) ) ;
#1757 = ORIENTED_EDGE ( 'NONE', *, *, #3553, .T. ) ;
#1758 = ORIENTED_EDGE ( 'NONE', *, *, #1677, .F. ) ;
#1759 = AXIS2_PLACEMENT_3D ( 'NONE', #3147, #6140, #7751 ) ;
#1760 = ORIENTED_EDGE ( 'NONE', *, *, #1820, .T. ) ;
#1761 = DIRECTION ( 'NONE',  ( 0.000000000000000000, 1.000000000000000000, 0.000000000000000000 ) ) ;
#1762 = CARTESIAN_POINT ( 'NONE',  ( -20.63749999999999929, 0.000000000000000000, 0.000000000000000000 ) ) ;
#1763 = LINE ( 'NONE', #5342, #6614 ) ;
#1764 = DIRECTION ( 'NONE',  ( 0.000000000000000000, 0.000000000000000000, 1.000000000000000000 ) ) ;
#1765 = LINE ( 'NONE', #2398, #5008 ) ;
#1766 = CIRCLE ( 'NONE', #7416, 5.000000000000000888 ) ;
#1767 = CARTESIAN_POINT ( 'NONE',  ( -29.99999999999999289, 3.673940397442058389E-15, -139.9999999999999716 ) ) ;
#1768 = ORIENTED_EDGE ( 'NONE', *, *, #4275, .F. ) ;
#1769 = ORIENTED_EDGE ( 'NONE', *, *, #5929, .T. ) ;
#1770 = VECTOR ( 'NONE', #5434, 1000.000000000000000 ) ;
#1771 = CARTESIAN_POINT ( 'NONE',  ( 4.339467034331189410, 6.732211846623394891, -4.700000000000006395 ) ) ;
#1772 = EDGE_CURVE ( 'NONE', #154, #5402, #5005, .T. ) ;
#1773 = PLANE ( 'NONE',  #4137 ) ;
#1774 = DIRECTION ( 'NONE',  ( -0.000000000000000000, -0.000000000000000000, 1.000000000000000000 ) ) ;
#1775 = CARTESIAN_POINT ( 'NONE',  ( 0.000000000000000000, 0.000000000000000000, 0.000000000000000000 ) ) ;
#1776 = FACE_OUTER_BOUND ( 'NONE', #6687, .T. ) ;
#1777 = CARTESIAN_POINT ( 'NONE',  ( 4.000000000000005329, -6.928203230275506108, 0.000000000000000000 ) ) ;
#1778 = EDGE_CURVE ( 'NONE', #2866, #4859, #6018, .T. ) ;
#1779 = EDGE_LOOP ( 'NONE', ( #2401, #4296, #6441, #5600 ) ) ;
#1780 = EDGE_CURVE ( 'NONE', #5051, #371, #7019, .T. ) ;
#1781 = ORIENTED_EDGE ( 'NONE', *, *, #453, .F. ) ;
#1782 = ORIENTED_EDGE ( 'NONE', *, *, #3398, .F. ) ;
#1783 = VECTOR ( 'NONE', #3241, 1000.000000000000000 ) ;
#1784 = CARTESIAN_POINT ( 'NONE',  ( -213.0929183184020701, 119.9981648402869467, -8.673617379884035472E-15 ) ) ;
#1785 = CARTESIAN_POINT ( 'NONE',  ( -68.76644452187068168, 49.96174644486002592, -40.00000000000000000 ) ) ;
#1786 =( NAMED_UNIT ( * ) PLANE_ANGLE_UNIT ( ) SI_UNIT ( $, .RADIAN. ) );
#1787 = DIRECTION ( 'NONE',  ( -0.000000000000000000, -0.000000000000000000, -1.000000000000000000 ) ) ;
#1788 = EDGE_CURVE ( 'NONE', #7134, #3642, #3372, .T. ) ;
#1789 = VERTEX_POINT ( 'NONE', #3813 ) ;
#1790 = AXIS2_PLACEMENT_3D ( 'NONE', #3511, #4728, #4769 ) ;
#1791 = ORIENTED_EDGE ( 'NONE', *, *, #84, .F. ) ;
#1792 = PLANE ( 'NONE',  #3043 ) ;
#1793 = FACE_OUTER_BOUND ( 'NONE', #7600, .T. ) ;
#1794 = DIRECTION ( 'NONE',  ( -0.000000000000000000, -0.000000000000000000, 1.000000000000000000 ) ) ;
#1795 = EDGE_LOOP ( 'NONE', ( #6378, #2655, #4106, #3165 ) ) ;
#1796 = ORIENTED_EDGE ( 'NONE', *, *, #7701, .T. ) ;
#1797 = ORIENTED_EDGE ( 'NONE', *, *, #32, .T. ) ;
#1798 = DIRECTION ( 'NONE',  ( 1.000000000000000000, 0.000000000000000000, 0.000000000000000000 ) ) ;
#1799 = DIRECTION ( 'NONE',  ( -0.000000000000000000, -0.000000000000000000, -1.000000000000000000 ) ) ;
#1800 = LINE ( 'NONE', #527, #2639 ) ;
#1801 = CARTESIAN_POINT ( 'NONE',  ( -8.000000000000000000, 0.000000000000000000, -4.700000000000000178 ) ) ;
#1802 = AXIS2_PLACEMENT_3D ( 'NONE', #96, #2515, #4908 ) ;
#1803 = CARTESIAN_POINT ( 'NONE',  ( -68.76644452187068168, 49.96174644486002592, 24.17200000000001125 ) ) ;
#1804 = ORIENTED_EDGE ( 'NONE', *, *, #5568, .T. ) ;
#1805 = EDGE_LOOP ( 'NONE', ( #7004, #6633, #7255, #3673 ) ) ;
#1806 = AXIS2_PLACEMENT_3D ( 'NONE', #7147, #3053, #3558 ) ;
#1807 = DIRECTION ( 'NONE',  ( -0.000000000000000000, -0.000000000000000000, 1.000000000000000000 ) ) ;
#1808 = CARTESIAN_POINT ( 'NONE',  ( -63.76644452187068879, 49.96174644486002592, 0.000000000000000000 ) ) ;
#1809 = DIRECTION ( 'NONE',  ( 1.000000000000000000, 0.000000000000000000, 0.000000000000000000 ) ) ;
#1810 = DIRECTION ( 'NONE',  ( 1.000000000000000000, 0.000000000000000000, 0.000000000000000000 ) ) ;
#1811 = CARTESIAN_POINT ( 'NONE',  ( -68.76644452187028378, -49.96174644486062277, -54.70000000000000284 ) ) ;
#1812 = LINE ( 'NONE', #6030, #4780 ) ;
#1813 = AXIS2_PLACEMENT_3D ( 'NONE', #2584, #1271, #3723 ) ;
#1814 = VERTEX_POINT ( 'NONE', #1036 ) ;
#1815 = ORIENTED_EDGE ( 'NONE', *, *, #4850, .F. ) ;
#1816 = ORIENTED_EDGE ( 'NONE', *, *, #1788, .F. ) ;
#1817 = CARTESIAN_POINT ( 'NONE',  ( 0.000000000000000000, 0.000000000000000000, 19.04999999999997229 ) ) ;
#1818 = CARTESIAN_POINT ( 'NONE',  ( -4.000000000000004441, -6.928203230275506108, -4.700000000000000178 ) ) ;
#1819 =( NAMED_UNIT ( * ) PLANE_ANGLE_UNIT ( ) SI_UNIT ( $, .RADIAN. ) );
#1820 = EDGE_CURVE ( 'NONE', #4328, #2865, #221, .T. ) ;
#1821 = DIRECTION ( 'NONE',  ( 0.9845265360683707057, 0.1752355551171480841, 0.000000000000000000 ) ) ;
#1822 = AXIS2_PLACEMENT_3D ( 'NONE', #631, #1407, #7483 ) ;
#1823 = ORIENTED_EDGE ( 'NONE', *, *, #632, .T. ) ;
#1824 = AXIS2_PLACEMENT_3D ( 'NONE', #5094, #2113, #6402 ) ;
#1825 = ORIENTED_EDGE ( 'NONE', *, *, #5000, .F. ) ;
#1826 = EDGE_CURVE ( 'NONE', #6698, #5437, #6525, .T. ) ;
#1827 = DIRECTION ( 'NONE',  ( 0.9938725510941108787, -0.1105321318969463978, 0.000000000000000000 ) ) ;
#1828 = AXIS2_PLACEMENT_3D ( 'NONE', #331, #289, #5030 ) ;
#1829 =( GEOMETRIC_REPRESENTATION_CONTEXT ( 3 ) GLOBAL_UNCERTAINTY_ASSIGNED_CONTEXT ( ( #5575 ) ) GLOBAL_UNIT_ASSIGNED_CONTEXT ( ( #1673, #4456, #2724 ) ) REPRESENTATION_CONTEXT ( 'NONE', 'WORKASPACE' ) );
#1830 = EDGE_CURVE ( 'NONE', #1298, #1609, #4113, .T. ) ;
#1831 = PLANE ( 'NONE',  #3254 ) ;
#1832 = CARTESIAN_POINT ( 'NONE',  ( 11.50644898236017433, -35.69105814929478981, -3.000000000000000000 ) ) ;
#1833 = ORIENTED_EDGE ( 'NONE', *, *, #400, .F. ) ;
#1834 = AXIS2_PLACEMENT_3D ( 'NONE', #4310, #5536, #5389 ) ;
#1835 = EDGE_CURVE ( 'NONE', #1985, #1532, #2381, .T. ) ;
#1836 = EDGE_LOOP ( 'NONE', ( #6987, #7334, #5728, #1982, #4147, #7079 ) ) ;
#1837 = PRODUCT ( 'torque nut 08_iso_ISO 10511-M10-N', 'torque nut 08_iso_ISO 10511-M10-N', '', ( #3258 ) ) ;
#1838 = DIRECTION ( 'NONE',  ( -0.000000000000000000, -0.000000000000000000, -1.000000000000000000 ) ) ;
#1839 = DIRECTION ( 'NONE',  ( 1.000000000000000000, 0.000000000000000000, 0.000000000000000000 ) ) ;
#1840 = PLANE ( 'NONE',  #2011 ) ;
#1841 = CARTESIAN_POINT ( 'NONE',  ( -3.500000000000006661, 0.000000000000000000, -32.25000000000000000 ) ) ;
#1842 = ADVANCED_FACE ( 'NONE', ( #5853 ), #4444, .F. ) ;
#1843 = AXIS2_PLACEMENT_3D ( 'NONE', #1207, #3656, #3622 ) ;
#1844 = CARTESIAN_POINT ( 'NONE',  ( -3.500000000000006661, 0.000000000000000000, 0.000000000000000000 ) ) ;
#1845 = ORIENTED_EDGE ( 'NONE', *, *, #1140, .F. ) ;
#1846 = DIRECTION ( 'NONE',  ( -1.000000000000000000, 0.000000000000000000, 0.000000000000000000 ) ) ;
#1847 = FACE_BOUND ( 'NONE', #2961, .T. ) ;
#1848 = DIRECTION ( 'NONE',  ( 0.9938725510941107677, -0.1105321318969463978, 0.000000000000000000 ) ) ;
#1849 = CARTESIAN_POINT ( 'NONE',  ( 46.38600551860989185, 165.3429183184012459, 0.000000000000000000 ) ) ;
#1850 = CARTESIAN_POINT ( 'NONE',  ( -4.586480920263581673, -37.21846574978686562, -3.000000000000000000 ) ) ;
#1851 = UNCERTAINTY_MEASURE_WITH_UNIT (LENGTH_MEASURE( 1.000000000000000082E-05 ), #347, 'distance_accuracy_value', 'NONE');
#1852 = CARTESIAN_POINT ( 'NONE',  ( 3.500000000000007550, 0.000000000000000000, -30.30000000000000071 ) ) ;
#1853 = ORIENTED_EDGE ( 'NONE', *, *, #4625, .T. ) ;
#1854 = VERTEX_POINT ( 'NONE', #4156 ) ;
#1855 = AXIS2_PLACEMENT_3D ( 'NONE', #758, #6837, #3764 ) ;
#1856 = ORIENTED_EDGE ( 'NONE', *, *, #1236, .T. ) ;
#1857 = CARTESIAN_POINT ( 'NONE',  ( 37.49999999999997868, 0.000000000000000000, -82.99999999999998579 ) ) ;
#1858 =( NAMED_UNIT ( * ) PLANE_ANGLE_UNIT ( ) SI_UNIT ( $, .RADIAN. ) );
#1859 = DIRECTION ( 'NONE',  ( 1.000000000000000000, 0.000000000000000000, 0.000000000000000000 ) ) ;
#1860 = AXIS2_PLACEMENT_3D ( 'NONE', #6408, #7540, #1549 ) ;
#1861 = EDGE_LOOP ( 'NONE', ( #4404, #1558 ) ) ;
#1862 = ORIENTED_EDGE ( 'NONE', *, *, #315, .F. ) ;
#1863 = CARTESIAN_POINT ( 'NONE',  ( 0.000000000000000000, 0.000000000000000000, -90.00000000000000000 ) ) ;
#1864 = ADVANCED_FACE ( 'NONE', ( #1156 ), #528, .F. ) ;
#1865 = CARTESIAN_POINT ( 'NONE',  ( -1.313474075707227851, -8.479269695850861766, -0.3167204509598428586 ) ) ;
#1866 = CYLINDRICAL_SURFACE ( 'NONE', #277, 5.250000000000004441 ) ;
#1867 = ADVANCED_FACE ( 'NONE', ( #444 ), #2903, .T. ) ;
#1868 = VERTEX_POINT ( 'NONE', #5893 ) ;
#1869 = EDGE_CURVE ( 'NONE', #3231, #2154, #2875, .T. ) ;
#1870 = CIRCLE ( 'NONE', #3126, 40.00000000000000711 ) ;
#1871 = EDGE_CURVE ( 'NONE', #3192, #952, #1765, .T. ) ;
#1872 = ORIENTED_EDGE ( 'NONE', *, *, #7071, .T. ) ;
#1873 = CARTESIAN_POINT ( 'NONE',  ( -207.8429183184026670, 119.9981648402859378, -50.00000000000000000 ) ) ;
#1874 = DIRECTION ( 'NONE',  ( 1.000000000000000000, 0.000000000000000000, 0.000000000000000000 ) ) ;
#1875 = TOROIDAL_SURFACE ( 'NONE', #3766, 30.30000000000000071, 0.3000000000000003775 ) ;
#1876 = FACE_BOUND ( 'NONE', #2789, .T. ) ;
#1877 = LINE ( 'NONE', #4905, #4756 ) ;
#1878 = ITEM_DEFINED_TRANSFORMATION ( 'NONE', 'NONE', #4942,  #7485 ) ;
#1879 = DIRECTION ( 'NONE',  ( 0.000000000000000000, 0.000000000000000000, 1.000000000000000000 ) ) ;
#1880 = ADVANCED_FACE ( 'NONE', ( #6413 ), #4707, .F. ) ;
#1881 = ORIENTED_EDGE ( 'NONE', *, *, #6017, .F. ) ;
#1882 = VECTOR ( 'NONE', #6026, 1000.000000000000000 ) ;
#1883 = CARTESIAN_POINT ( 'NONE',  ( 10.00000000000000000, 33.54101966249685773, -60.00000000000000711 ) ) ;
#1884 = AXIS2_PLACEMENT_3D ( 'NONE', #5222, #5300, #2860 ) ;
#1885 = CARTESIAN_POINT ( 'NONE',  ( -1.791896790581761989, 35.93034554373089406, -119.9999999999999858 ) ) ;
#1886 = DIRECTION ( 'NONE',  ( 1.000000000000000000, 0.000000000000000000, 0.000000000000000000 ) ) ;
#1887 = DIRECTION ( 'NONE',  ( 0.000000000000000000, 0.000000000000000000, 1.000000000000000000 ) ) ;
#1888 = FILL_AREA_STYLE ('',( #5313 ) ) ;
#1889 = CARTESIAN_POINT ( 'NONE',  ( -29.99999999999999289, 3.673940397442058389E-15, -139.9999999999999716 ) ) ;
#1890 = DIRECTION ( 'NONE',  ( 0.8571673007021121116, 1.049727191138618449E-16, -0.5150380749100544886 ) ) ;
#1891 = ORIENTED_EDGE ( 'NONE', *, *, #394, .F. ) ;
#1892 = EDGE_LOOP ( 'NONE', ( #7570, #7268, #5159, #7586 ) ) ;
#1893 = ORIENTED_EDGE ( 'NONE', *, *, #2312, .T. ) ;
#1894 = DIRECTION ( 'NONE',  ( 0.000000000000000000, 0.000000000000000000, -1.000000000000000000 ) ) ;
#1895 =( LENGTH_UNIT ( ) NAMED_UNIT ( * ) SI_UNIT ( .MILLI., .METRE. ) );
#1896 = AXIS2_PLACEMENT_3D ( 'NONE', #5747, #6860, #1605 ) ;
#1897 = DIRECTION ( 'NONE',  ( -3.081487911019577365E-33, 2.775557561562891967E-17, 1.000000000000000000 ) ) ;
#1898 = PRODUCT_DEFINITION_SHAPE ( 'NONE', 'NONE',  #7797 ) ;
#1899 = ORIENTED_EDGE ( 'NONE', *, *, #4315, .F. ) ;
#1900 = ORIENTED_EDGE ( 'NONE', *, *, #3757, .T. ) ;
#1901 = CIRCLE ( 'NONE', #6681, 35.00000000000000711 ) ;
#1902 = DIRECTION ( 'NONE',  ( 1.000000000000000000, 0.000000000000000000, 0.000000000000000000 ) ) ;
#1903 = CARTESIAN_POINT ( 'NONE',  ( 9.568665290872615969, -28.43309066125680928, -122.9999999999999716 ) ) ;
#1904 = AXIS2_PLACEMENT_3D ( 'NONE', #1535, #5639, #233 ) ;
#1905 = CARTESIAN_POINT ( 'NONE',  ( -68.76644452187068168, 49.96174644486002592, 0.000000000000000000 ) ) ;
#1906 = EDGE_LOOP ( 'NONE', ( #7125, #6227, #1640, #4041 ) ) ;
#1907 = VERTEX_POINT ( 'NONE', #1116 ) ;
#1908 = CIRCLE ( 'NONE', #6319, 28.49999999999999645 ) ;
#1909 = CARTESIAN_POINT ( 'NONE',  ( 0.000000000000000000, 0.000000000000000000, -82.99999999999995737 ) ) ;
#1910 = DIRECTION ( 'NONE',  ( -0.000000000000000000, -0.000000000000000000, 1.000000000000000000 ) ) ;
#1911 = DIRECTION ( 'NONE',  ( 0.000000000000000000, 0.000000000000000000, 1.000000000000000000 ) ) ;
#1912 = CARTESIAN_POINT ( 'NONE',  ( 0.000000000000000000, 0.000000000000000000, -3.000000000000000000 ) ) ;
#1913 = CONTEXT_DEPENDENT_SHAPE_REPRESENTATION ( #3753, #4977 ) ;
#1914 = EDGE_CURVE ( 'NONE', #7003, #7044, #2622, .T. ) ;
#1915 = DIRECTION ( 'NONE',  ( 1.000000000000000000, 0.000000000000000000, 0.000000000000000000 ) ) ;
#1916 = ORIENTED_EDGE ( 'NONE', *, *, #7217, .T. ) ;
#1917 = DIRECTION ( 'NONE',  ( 0.000000000000000000, 0.000000000000000000, -1.000000000000000000 ) ) ;
#1918 = EDGE_CURVE ( 'NONE', #6794, #5950, #3755, .T. ) ;
#1919 = DIRECTION ( 'NONE',  ( 0.000000000000000000, 0.000000000000000000, 1.000000000000000000 ) ) ;
#1920 = DIRECTION ( 'NONE',  ( 1.000000000000000000, 0.000000000000000000, 0.000000000000000000 ) ) ;
#1921 = APPLICATION_PROTOCOL_DEFINITION ( 'draft international standard', 'automotive_design', 1998, #6770 ) ;
#1922 = DIRECTION ( 'NONE',  ( 0.000000000000000000, -1.224646799147352961E-16, 1.000000000000000000 ) ) ;
#1923 = FACE_OUTER_BOUND ( 'NONE', #3523, .T. ) ;
#1924 = DIRECTION ( 'NONE',  ( 0.000000000000000000, 0.000000000000000000, 1.000000000000000000 ) ) ;
#1925 = EDGE_LOOP ( 'NONE', ( #634, #519, #6187, #1744, #3454, #6306 ) ) ;
#1926 = AXIS2_PLACEMENT_3D ( 'NONE', #4028, #6440, #1023 ) ;
#1927 = DIRECTION ( 'NONE',  ( 0.000000000000000000, 0.000000000000000000, -1.000000000000000000 ) ) ;
#1928 = ORIENTED_EDGE ( 'NONE', *, *, #1486, .F. ) ;
#1929 = EDGE_CURVE ( 'NONE', #5275, #2430, #5638, .T. ) ;
#1930 = VERTEX_POINT ( 'NONE', #6447 ) ;
#1931 = DIRECTION ( 'NONE',  ( 0.000000000000000000, 0.000000000000000000, 1.000000000000000000 ) ) ;
#1932 = CARTESIAN_POINT ( 'NONE',  ( -105.4635834177243936, 106.6650485055563990, 5.000000000000000000 ) ) ;
#1933 =( LENGTH_UNIT ( ) NAMED_UNIT ( * ) SI_UNIT ( .MILLI., .METRE. ) );
#1934 = AXIS2_PLACEMENT_3D ( 'NONE', #1946, #5608, #3834 ) ;
#1935 =( GEOMETRIC_REPRESENTATION_CONTEXT ( 3 ) GLOBAL_UNCERTAINTY_ASSIGNED_CONTEXT ( ( #7220 ) ) GLOBAL_UNIT_ASSIGNED_CONTEXT ( ( #6776, #5624, #1436 ) ) REPRESENTATION_CONTEXT ( 'NONE', 'WORKASPACE' ) );
#1936 = DIRECTION ( 'NONE',  ( -0.000000000000000000, -0.000000000000000000, 1.000000000000000000 ) ) ;
#1937 = EDGE_CURVE ( 'NONE', #6826, #2604, #7650, .T. ) ;
#1938 = EDGE_LOOP ( 'NONE', ( #464, #4811, #3806, #503, #3845, #333 ) ) ;
#1939 = ORIENTED_EDGE ( 'NONE', *, *, #3219, .F. ) ;
#1940 = ORIENTED_EDGE ( 'NONE', *, *, #2645, .F. ) ;
#1941 = VECTOR ( 'NONE', #7153, 1000.000000000000000 ) ;
#1942 = DIRECTION ( 'NONE',  ( 1.000000000000000000, 0.000000000000000000, 0.000000000000000000 ) ) ;
#1943 = LINE ( 'NONE', #3087, #58 ) ;
#1944 = CARTESIAN_POINT ( 'NONE',  ( -68.76644452187068168, 49.96174644486002592, 24.17200000000001125 ) ) ;
#1945 = CIRCLE ( 'NONE', #290, 4.171999999999995268 ) ;
#1946 = CARTESIAN_POINT ( 'NONE',  ( 0.000000000000000000, 0.000000000000000000, -82.99999999999998579 ) ) ;
#1947 = VERTEX_POINT ( 'NONE', #2982 ) ;
#1948 = VERTEX_POINT ( 'NONE', #3529 ) ;
#1949 = CIRCLE ( 'NONE', #6101, 35.97500000000000142 ) ;
#1950 = CIRCLE ( 'NONE', #557, 5.249999999999977796 ) ;
#1951 = CARTESIAN_POINT ( 'NONE',  ( 39.64284999284935651, -144.6666666666667140, 10.00000000000000000 ) ) ;
#1952 = DIRECTION ( 'NONE',  ( 1.000000000000000000, 0.000000000000000000, 0.000000000000000000 ) ) ;
#1953 = FACE_OUTER_BOUND ( 'NONE', #3916, .T. ) ;
#1954 = DIRECTION ( 'NONE',  ( 1.000000000000000000, 0.000000000000000000, 0.000000000000000000 ) ) ;
#1955 = ITEM_DEFINED_TRANSFORMATION ( 'NONE', 'NONE', #7464,  #7485 ) ;
#1956 = UNCERTAINTY_MEASURE_WITH_UNIT (LENGTH_MEASURE( 1.000000000000000082E-05 ), #5597, 'distance_accuracy_value', 'NONE');
#1957 = CARTESIAN_POINT ( 'NONE',  ( -1.499999999999999334, -33.63777638310832430, -3.000000000000000000 ) ) ;
#1958 = EDGE_CURVE ( 'NONE', #4364, #7642, #341, .T. ) ;
#1959 = VECTOR ( 'NONE', #4709, 1000.000000000000000 ) ;
#1960 = ORIENTED_EDGE ( 'NONE', *, *, #1778, .F. ) ;
#1961 = FACE_OUTER_BOUND ( 'NONE', #7585, .T. ) ;
#1962 = CARTESIAN_POINT ( 'NONE',  ( -129.9038105676659995, 74.99999999999971578, 10.00000000000000000 ) ) ;
#1963 = LINE ( 'NONE', #3887, #5776 ) ;
#1964 = DIRECTION ( 'NONE',  ( 0.000000000000000000, 0.000000000000000000, -1.000000000000000000 ) ) ;
#1965 = APPLICATION_PROTOCOL_DEFINITION ( 'draft international standard', 'automotive_design', 1998, #4595 ) ;
#1966 = PRODUCT_DEFINITION_SHAPE ( 'NONE', 'NONE',  #7782 ) ;
#1967 = PLANE ( 'NONE',  #1570 ) ;
#1968 = EDGE_CURVE ( 'NONE', #3701, #2140, #7000, .T. ) ;
#1969 = CARTESIAN_POINT ( 'NONE',  ( 4.000000000000000000, -33.63777638310832430, 0.000000000000000000 ) ) ;
#1970 = DIRECTION ( 'NONE',  ( 1.000000000000000000, 0.000000000000000000, 0.000000000000000000 ) ) ;
#1971 = EDGE_CURVE ( 'NONE', #6313, #3054, #3505, .T. ) ;
#1972 = VERTEX_POINT ( 'NONE', #7276 ) ;
#1973 = EDGE_CURVE ( 'NONE', #1053, #1854, #5260, .T. ) ;
#1974 = VERTEX_POINT ( 'NONE', #1841 ) ;
#1975 = ADVANCED_FACE ( 'NONE', ( #3140, #3178, #54, #7239, #6173, #6648 ), #4270, .T. ) ;
#1976 = EDGE_LOOP ( 'NONE', ( #3215, #1853, #5616, #5995 ) ) ;
#1977 =( GEOMETRIC_REPRESENTATION_CONTEXT ( 3 ) GLOBAL_UNCERTAINTY_ASSIGNED_CONTEXT ( ( #6684 ) ) GLOBAL_UNIT_ASSIGNED_CONTEXT ( ( #2818, #4151, #1593 ) ) REPRESENTATION_CONTEXT ( 'NONE', 'WORKASPACE' ) );
#1978 = CARTESIAN_POINT ( 'NONE',  ( 8.000000000000000000, 4.618802153517013842, -3.985468820183668104 ) ) ;
#1979 =( LENGTH_UNIT ( ) NAMED_UNIT ( * ) SI_UNIT ( .MILLI., .METRE. ) );
#1980 = CARTESIAN_POINT ( 'NONE',  ( -199.9963296805737230, 0.000000000000000000, 0.000000000000000000 ) ) ;
#1981 = EDGE_CURVE ( 'NONE', #4626, #5051, #647, .T. ) ;
#1982 = ORIENTED_EDGE ( 'NONE', *, *, #3025, .F. ) ;
#1983 = VERTEX_POINT ( 'NONE', #1801 ) ;
#1984 = AXIS2_PLACEMENT_3D ( 'NONE', #4385, #5723, #3176 ) ;
#1985 = VERTEX_POINT ( 'NONE', #3725 ) ;
#1986 = DIRECTION ( 'NONE',  ( 0.000000000000000000, 0.000000000000000000, 1.000000000000000000 ) ) ;
#1987 = CARTESIAN_POINT ( 'NONE',  ( 0.000000000000000000, 0.000000000000000000, 0.000000000000000000 ) ) ;
#1988 = CIRCLE ( 'NONE', #4241, 32.49999999999997158 ) ;
#1989 = LINE ( 'NONE', #6240, #2389 ) ;
#1990 = CARTESIAN_POINT ( 'NONE',  ( -3.200000000000007727, 0.000000000000000000, -30.30000000000000071 ) ) ;
#1991 = ORIENTED_EDGE ( 'NONE', *, *, #2405, .F. ) ;
#1992 =( REPRESENTATION_RELATIONSHIP ('NONE','NONE', #1229, #1433 ) REPRESENTATION_RELATIONSHIP_WITH_TRANSFORMATION ( #6962 )SHAPE_REPRESENTATION_RELATIONSHIP( ) );
#1993 = DIRECTION ( 'NONE',  ( 1.000000000000000000, 0.000000000000000000, 0.000000000000000000 ) ) ;
#1994 = DIRECTION ( 'NONE',  ( -0.000000000000000000, -0.000000000000000000, 1.000000000000000000 ) ) ;
#1995 = DIRECTION ( 'NONE',  ( 0.1305261922200541547, 0.9914448613738101601, -0.000000000000000000 ) ) ;
#1996 = AXIS2_PLACEMENT_3D ( 'NONE', #2323, #6569, #571 ) ;
#1997 = LINE ( 'NONE', #2586, #3811 ) ;
#1998 = EDGE_LOOP ( 'NONE', ( #2681, #1447, #3493, #1768 ) ) ;
#1999 = LINE ( 'NONE', #3182, #1730 ) ;
#2000 = VECTOR ( 'NONE', #436, 1000.000000000000000 ) ;
#2001 = CARTESIAN_POINT ( 'NONE',  ( -3.200000000000007727, 0.000000000000000000, 0.000000000000000000 ) ) ;
#2002 = CARTESIAN_POINT ( 'NONE',  ( 10.69810649761387822, -28.02767413407169528, -122.9999999999999716 ) ) ;
#2003 = CARTESIAN_POINT ( 'NONE',  ( -1.852913429038039572, -299.9999999999999432, -82.99999999999998579 ) ) ;
#2004 = AXIS2_PLACEMENT_3D ( 'NONE', #4562, #7128, #2833 ) ;
#2005 = CARTESIAN_POINT ( 'NONE',  ( 3.319543390096038493, -7.321065037175432444, -4.683111142572228935 ) ) ;
#2006 = DIRECTION ( 'NONE',  ( 1.000000000000000000, 0.000000000000000000, 0.000000000000000000 ) ) ;
#2007 = ORIENTED_EDGE ( 'NONE', *, *, #1480, .T. ) ;
#2008 = AXIS2_PLACEMENT_3D ( 'NONE', #6798, #785, #2652 ) ;
#2009 = ORIENTED_EDGE ( 'NONE', *, *, #1619, .T. ) ;
#2010 = ORIENTED_EDGE ( 'NONE', *, *, #2687, .F. ) ;
#2011 = AXIS2_PLACEMENT_3D ( 'NONE', #4904, #3569, #6608 ) ;
#2012 = EDGE_CURVE ( 'NONE', #6651, #4919, #7524, .T. ) ;
#2013 = ORIENTED_EDGE ( 'NONE', *, *, #2459, .T. ) ;
#2014 = CARTESIAN_POINT ( 'NONE',  ( 0.000000000000000000, 0.000000000000000000, -3.000000000000000000 ) ) ;
#2015 = FILL_AREA_STYLE ('',( #3823 ) ) ;
#2016 = SURFACE_SIDE_STYLE ('',( #4527 ) ) ;
#2017 = EDGE_CURVE ( 'NONE', #2536, #3380, #2513, .T. ) ;
#2018 = LINE ( 'NONE', #932, #4711 ) ;
#2019 = AXIS2_PLACEMENT_3D ( 'NONE', #1736, #4836, #4209 ) ;
#2020 = ADVANCED_FACE ( 'NONE', ( #3059 ), #5459, .F. ) ;
#2021 = ORIENTED_EDGE ( 'NONE', *, *, #6504, .F. ) ;
#2022 = ORIENTED_EDGE ( 'NONE', *, *, #2069, .F. ) ;
#2023 = AXIS2_PLACEMENT_3D ( 'NONE', #548, #6550, #6508 ) ;
#2024 = DIRECTION ( 'NONE',  ( -0.000000000000000000, -0.000000000000000000, 1.000000000000000000 ) ) ;
#2025 = EDGE_CURVE ( 'NONE', #5644, #2609, #1877, .T. ) ;
#2026 = FILL_AREA_STYLE ('',( #1458 ) ) ;
#2027 = DIRECTION ( 'NONE',  ( 0.000000000000000000, 0.000000000000000000, -1.000000000000000000 ) ) ;
#2028 = CARTESIAN_POINT ( 'NONE',  ( 3.660532965668821692, -7.124194613927628872, -3.335192229813806599E-16 ) ) ;
#2029 = ORIENTED_EDGE ( 'NONE', *, *, #3174, .T. ) ;
#2030 = AXIS2_PLACEMENT_3D ( 'NONE', #6230, #1331, #7296 ) ;
#2031 = PRODUCT_DEFINITION_SHAPE ( 'NONE', 'NONE',  #7802 ) ;
#2032 = CARTESIAN_POINT ( 'NONE',  ( 5.870234470492294880E-31, -4.203179568131150526E-15, -122.9999999999999716 ) ) ;
#2033 = CARTESIAN_POINT ( 'NONE',  ( 0.000000000000000000, 0.000000000000000000, -50.00000000000000000 ) ) ;
#2034 = AXIS2_PLACEMENT_3D ( 'NONE', #4694, #3597, #3010 ) ;
#2035 = DIRECTION ( 'NONE',  ( 1.000000000000000000, 0.000000000000000000, 0.000000000000000000 ) ) ;
#2036 = CYLINDRICAL_SURFACE ( 'NONE', #779, 28.50000000000000711 ) ;
#2037 = EDGE_CURVE ( 'NONE', #1572, #2635, #1870, .T. ) ;
#2038 = EDGE_LOOP ( 'NONE', ( #1343, #7627, #6479, #3190, #708, #7738 ) ) ;
#2039 = AXIS2_PLACEMENT_3D ( 'NONE', #2456, #4843, #7256 ) ;
#2040 = APPLICATION_CONTEXT ( 'automotive_design' ) ;
#2041 = DIRECTION ( 'NONE',  ( 1.000000000000000000, 0.000000000000000000, -0.000000000000000000 ) ) ;
#2042 = DIRECTION ( 'NONE',  ( -0.000000000000000000, -0.000000000000000000, 1.000000000000000000 ) ) ;
#2043 = DIRECTION ( 'NONE',  ( 1.000000000000000000, 0.000000000000000000, 0.000000000000000000 ) ) ;
#2044 = LINE ( 'NONE', #4437, #2119 ) ;
#2045 = DIRECTION ( 'NONE',  ( -0.05019371822566820462, 0.9987395008963457776, -2.550145071705742900E-17 ) ) ;
#2046 = DIRECTION ( 'NONE',  ( 1.000000000000000000, 0.000000000000000000, 0.000000000000000000 ) ) ;
#2047 = CARTESIAN_POINT ( 'NONE',  ( -125.2481648402875578, 207.8429183184017859, -50.00000000000000000 ) ) ;
#2048 = ORIENTED_EDGE ( 'NONE', *, *, #5769, .T. ) ;
#2049 = VERTEX_POINT ( 'NONE', #3021 ) ;
#2050 = ORIENTED_EDGE ( 'NONE', *, *, #7020, .T. ) ;
#2051 = SHAPE_REPRESENTATION ( 'stud', ( #7485 ), #2832 ) ;
#2052 = ORIENTED_EDGE ( 'NONE', *, *, #5481, .F. ) ;
#2053 = CARTESIAN_POINT ( 'NONE',  ( 26.26644452187122170, -80.83980388508783221, 10.00000000000000000 ) ) ;
#2054 = DIRECTION ( 'NONE',  ( 0.000000000000000000, 0.000000000000000000, 1.000000000000000000 ) ) ;
#2055 = CARTESIAN_POINT ( 'NONE',  ( 129.9038105676665396, -74.99999999999882050, 10.00000000000000000 ) ) ;
#2056 = AXIS2_PLACEMENT_3D ( 'NONE', #7616, #5215, #1626 ) ;
#2057 = EDGE_CURVE ( 'NONE', #6200, #3301, #2435, .T. ) ;
#2058 = VERTEX_POINT ( 'NONE', #6720 ) ;
#2059 = ORIENTED_EDGE ( 'NONE', *, *, #6746, .T. ) ;
#2060 = VECTOR ( 'NONE', #7733, 1000.000000000000000 ) ;
#2061 = EDGE_CURVE ( 'NONE', #7599, #4081, #1943, .T. ) ;
#2062 = CARTESIAN_POINT ( 'NONE',  ( 0.000000000000000000, 0.000000000000000000, 13.00000000000001066 ) ) ;
#2063 =( NAMED_UNIT ( * ) SI_UNIT ( $, .STERADIAN. ) SOLID_ANGLE_UNIT ( ) );
#2064 = FACE_OUTER_BOUND ( 'NONE', #6156, .T. ) ;
#2065 = DIRECTION ( 'NONE',  ( -0.3189555096957539804, 0.9477696887085605981, -2.581026109104742394E-17 ) ) ;
#2066 = AXIS2_PLACEMENT_3D ( 'NONE', #4110, #6014, #5422 ) ;
#2067 = VERTEX_POINT ( 'NONE', #6133 ) ;
#2068 = EDGE_CURVE ( 'NONE', #5644, #5391, #5127, .T. ) ;
#2069 = EDGE_CURVE ( 'NONE', #1601, #6833, #1199, .T. ) ;
#2070 = DIRECTION ( 'NONE',  ( -0.000000000000000000, -0.000000000000000000, 1.000000000000000000 ) ) ;
#2071 = DIRECTION ( 'NONE',  ( 0.000000000000000000, 0.000000000000000000, 1.000000000000000000 ) ) ;
#2072 = AXIS2_PLACEMENT_3D ( 'NONE', #1699, #3429, #7580 ) ;
#2073 = DIRECTION ( 'NONE',  ( 0.000000000000000000, 0.000000000000000000, 1.000000000000000000 ) ) ;
#2074 = ADVANCED_FACE ( 'NONE', ( #1273 ), #608, .T. ) ;
#2075 = DIRECTION ( 'NONE',  ( 0.9938725510941108787, -0.1105321318969463978, 0.000000000000000000 ) ) ;
#2076 = EDGE_LOOP ( 'NONE', ( #2825, #2305 ) ) ;
#2077 = EDGE_CURVE ( 'NONE', #3551, #4859, #5760, .T. ) ;
#2078 = AXIS2_PLACEMENT_3D ( 'NONE', #4306, #6717, #1310 ) ;
#2079 = FACE_BOUND ( 'NONE', #642, .T. ) ;
#2080 = DIRECTION ( 'NONE',  ( -0.000000000000000000, -0.000000000000000000, 1.000000000000000000 ) ) ;
#2081 = EDGE_CURVE ( 'NONE', #699, #1651, #1484, .T. ) ;
#2082 = PLANE ( 'NONE',  #108 ) ;
#2083 = CARTESIAN_POINT ( 'NONE',  ( -68.76644452187068168, 49.96174644486002592, 0.000000000000000000 ) ) ;
#2084 = APPLICATION_PROTOCOL_DEFINITION ( 'draft international standard', 'automotive_design', 1998, #7419 ) ;
#2085 = AXIS2_PLACEMENT_3D ( 'NONE', #7746, #3413, #6449 ) ;
#2086 =( GEOMETRIC_REPRESENTATION_CONTEXT ( 3 ) GLOBAL_UNCERTAINTY_ASSIGNED_CONTEXT ( ( #1313 ) ) GLOBAL_UNIT_ASSIGNED_CONTEXT ( ( #3527, #4891, #1154 ) ) REPRESENTATION_CONTEXT ( 'NONE', 'WORKASPACE' ) );
#2087 = PRESENTATION_STYLE_ASSIGNMENT (( #3776 ) ) ;
#2088 = VERTEX_POINT ( 'NONE', #5424 ) ;
#2089 = EDGE_LOOP ( 'NONE', ( #4022, #2498, #2483 ) ) ;
#2090 = ORIENTED_EDGE ( 'NONE', *, *, #1427, .T. ) ;
#2091 = AXIS2_PLACEMENT_3D ( 'NONE', #611, #648, #56 ) ;
#2092 = MECHANICAL_DESIGN_GEOMETRIC_PRESENTATION_REPRESENTATION (  '', ( #1577 ), #7375 ) ;
#2093 = ORIENTED_EDGE ( 'NONE', *, *, #7116, .F. ) ;
#2094 = DIRECTION ( 'NONE',  ( 0.000000000000000000, 0.000000000000000000, 1.000000000000000000 ) ) ;
#2095 = DIRECTION ( 'NONE',  ( 1.000000000000000000, -1.776356839400250465E-15, 0.000000000000000000 ) ) ;
#2096 =( NAMED_UNIT ( * ) SI_UNIT ( $, .STERADIAN. ) SOLID_ANGLE_UNIT ( ) );
#2097 = DIRECTION ( 'NONE',  ( 1.000000000000000000, 2.398081733190338127E-14, 0.000000000000000000 ) ) ;
#2098 = CLOSED_SHELL ( 'NONE', ( #2595, #3549, #7539, #2215, #6494, #3606, #852, #5190, #712, #7026, #1975, #5173, #1523, #1518, #3847, #1474 ) ) ;
#2099 = PRODUCT ( 'stud', 'stud', '', ( #6182 ) ) ;
#2100 = VERTEX_POINT ( 'NONE', #5496 ) ;
#2101 = ORIENTED_EDGE ( 'NONE', *, *, #4995, .T. ) ;
#2102 = CIRCLE ( 'NONE', #5874, 28.49999999999999645 ) ;
#2103 = ORIENTED_EDGE ( 'NONE', *, *, #3841, .T. ) ;
#2104 = DIRECTION ( 'NONE',  ( 1.000000000000000000, 0.000000000000000000, 0.000000000000000000 ) ) ;
#2105 = DIRECTION ( 'NONE',  ( 1.000000000000000000, 0.000000000000000000, 0.000000000000000000 ) ) ;
#2106 = AXIS2_PLACEMENT_3D ( 'NONE', #4658, #3518, #7027 ) ;
#2107 = CARTESIAN_POINT ( 'NONE',  ( 105.4635834177229157, 106.6650485055578770, 10.00000000000000000 ) ) ;
#2108 = ORIENTED_EDGE ( 'NONE', *, *, #5640, .T. ) ;
#2109 = AXIS2_PLACEMENT_3D ( 'NONE', #4677, #2408, #2333 ) ;
#2110 = EDGE_CURVE ( 'NONE', #5113, #3517, #476, .T. ) ;
#2111 = DIRECTION ( 'NONE',  ( 0.5000000000000101030, -0.8660254037844328234, 0.000000000000000000 ) ) ;
#2112 = B_SPLINE_CURVE_WITH_KNOTS ( 'NONE', 3,
 ( #6259, #2746, #2005, #5065, #3338, #2633, #3227, #1360 ),
 .UNSPECIFIED., .F., .F.,
 ( 4, 2, 2, 4 ),
 ( 0.004673709593152147908, 0.005837709341827642534, 0.007001709090503137160, 0.009329708587854127280 ),
 .UNSPECIFIED. ) ;
#2113 = DIRECTION ( 'NONE',  ( -0.000000000000000000, -0.000000000000000000, 1.000000000000000000 ) ) ;
#2114 = DIRECTION ( 'NONE',  ( -0.000000000000000000, -0.000000000000000000, -1.000000000000000000 ) ) ;
#2115 = EDGE_CURVE ( 'NONE', #1212, #520, #5890, .T. ) ;
#2116 = EDGE_CURVE ( 'NONE', #2383, #5846, #6206, .T. ) ;
#2117 = DIRECTION ( 'NONE',  ( -0.4999999999999918954, -0.8660254037844432595, 0.000000000000000000 ) ) ;
#2118 = ORIENTED_EDGE ( 'NONE', *, *, #419, .T. ) ;
#2119 = VECTOR ( 'NONE', #805, 1000.000000000000000 ) ;
#2120 = EDGE_CURVE ( 'NONE', #5661, #3942, #2739, .T. ) ;
#2121 = CARTESIAN_POINT ( 'NONE',  ( -37.49999999999997868, 0.000000000000000000, -119.9999999999999858 ) ) ;
#2122 = CARTESIAN_POINT ( 'NONE',  ( 0.000000000000000000, 0.000000000000000000, 0.000000000000000000 ) ) ;
#2123 = CIRCLE ( 'NONE', #7514, 35.00000000000000711 ) ;
#2124 = CARTESIAN_POINT ( 'NONE',  ( -5.134781488891348999E-13, 239.9963296805737230, -50.00000000000000000 ) ) ;
#2125 = CARTESIAN_POINT ( 'NONE',  ( 8.000000000000000000, 3.115336682267008772, -4.380606868608494686 ) ) ;
#2126 = DIRECTION ( 'NONE',  ( 1.000000000000000000, 0.000000000000000000, 0.000000000000000000 ) ) ;
#2127 = EDGE_CURVE ( 'NONE', #2919, #6450, #6804, .T. ) ;
#2128 = DIRECTION ( 'NONE',  ( -0.000000000000000000, -0.000000000000000000, 1.000000000000000000 ) ) ;
#2129 = VERTEX_POINT ( 'NONE', #3804 ) ;
#2130 = ORIENTED_EDGE ( 'NONE', *, *, #5621, .F. ) ;
#2131 = AXIS2_PLACEMENT_3D ( 'NONE', #1312, #3100, #2479 ) ;
#2132 = ORIENTED_EDGE ( 'NONE', *, *, #4820, .F. ) ;
#2133 = ORIENTED_EDGE ( 'NONE', *, *, #159, .T. ) ;
#2134 = CARTESIAN_POINT ( 'NONE',  ( -4.000000000000004441, 6.928203230275506108, 0.000000000000000000 ) ) ;
#2135 = CARTESIAN_POINT ( 'NONE',  ( -8.000000000000000000, 3.115336682266999446, -0.3193931313915043257 ) ) ;
#2136 = TOROIDAL_SURFACE ( 'NONE', #7290, 30.30000000000000071, 0.3000000000000003775 ) ;
#2137 = CARTESIAN_POINT ( 'NONE',  ( 114.7481648402869041, 207.8429183184021269, 10.00000000000000000 ) ) ;
#2138 = ORIENTED_EDGE ( 'NONE', *, *, #6395, .F. ) ;
#2139 = AXIS2_PLACEMENT_3D ( 'NONE', #2521, #4912, #1809 ) ;
#2140 = VERTEX_POINT ( 'NONE', #5725 ) ;
#2141 = ORIENTED_EDGE ( 'NONE', *, *, #6017, .T. ) ;
#2142 = FACE_OUTER_BOUND ( 'NONE', #2574, .T. ) ;
#2143 = SURFACE_STYLE_USAGE ( .BOTH. , #5641 ) ;
#2144 = CIRCLE ( 'NONE', #5652, 8.000000000000000000 ) ;
#2145 = DIRECTION ( 'NONE',  ( 0.000000000000000000, 0.000000000000000000, 1.000000000000000000 ) ) ;
#2146 =( REPRESENTATION_RELATIONSHIP ('NONE','NONE', #1229, #1433 ) REPRESENTATION_RELATIONSHIP_WITH_TRANSFORMATION ( #1350 )SHAPE_REPRESENTATION_RELATIONSHIP( ) );
#2147 = CARTESIAN_POINT ( 'NONE',  ( 4.000000000000004441, 6.928203230275507885, 0.000000000000000000 ) ) ;
#2148 = ORIENTED_EDGE ( 'NONE', *, *, #5326, .F. ) ;
#2149 = CARTESIAN_POINT ( 'NONE',  ( -9.702951051037022268, -29.86427928513813512, -3.000000000000000000 ) ) ;
#2150 = CARTESIAN_POINT ( 'NONE',  ( 21.01644452187054313, 80.83980388508807380, 10.00000000000000000 ) ) ;
#2151 = CARTESIAN_POINT ( 'NONE',  ( -4.000000000000004441, -6.928203230275506108, -4.700000000000000178 ) ) ;
#2152 = AXIS2_PLACEMENT_3D ( 'NONE', #1656, #7098, #5280 ) ;
#2153 = DIRECTION ( 'NONE',  ( 1.000000000000000000, 0.000000000000000000, 0.000000000000000000 ) ) ;
#2154 = VERTEX_POINT ( 'NONE', #2733 ) ;
#2155 = CARTESIAN_POINT ( 'NONE',  ( -350.0000000000000000, 37.15382499588017140, -1041.954445729288636 ) ) ;
#2156 = AXIS2_PLACEMENT_3D ( 'NONE', #5561, #1263, #673 ) ;
#2157 = CYLINDRICAL_SURFACE ( 'NONE', #6876, 35.00000000000000711 ) ;
#2158 = DIRECTION ( 'NONE',  ( 1.000000000000000000, 0.000000000000000000, 0.000000000000000000 ) ) ;
#2159 = EDGE_CURVE ( 'NONE', #4490, #1053, #6877, .T. ) ;
#2160 = DIRECTION ( 'NONE',  ( 1.000000000000000000, 0.000000000000000000, 0.000000000000000000 ) ) ;
#2161 = DIRECTION ( 'NONE',  ( 0.000000000000000000, 0.000000000000000000, 1.000000000000000000 ) ) ;
#2162 = DIRECTION ( 'NONE',  ( 1.000000000000000000, 0.000000000000000000, 0.000000000000000000 ) ) ;
#2163 = AXIS2_PLACEMENT_3D ( 'NONE', #5441, #3003, #5406 ) ;
#2164 = EDGE_LOOP ( 'NONE', ( #5033, #254, #1353, #2293 ) ) ;
#2165 = ORIENTED_EDGE ( 'NONE', *, *, #2938, .T. ) ;
#2166 = ORIENTED_EDGE ( 'NONE', *, *, #4271, .F. ) ;
#2167 = EDGE_CURVE ( 'NONE', #3380, #7398, #5515, .T. ) ;
#2168 = DIRECTION ( 'NONE',  ( 1.000000000000000000, 0.000000000000000000, 0.000000000000000000 ) ) ;
#2169 = FACE_OUTER_BOUND ( 'NONE', #5325, .T. ) ;
#2170 = ADVANCED_FACE ( 'NONE', ( #5614 ), #1355, .T. ) ;
#2171 = LINE ( 'NONE', #7085, #3144 ) ;
#2172 = LINE ( 'NONE', #2211, #753 ) ;
#2173 = DIRECTION ( 'NONE',  ( -0.000000000000000000, -0.000000000000000000, 1.000000000000000000 ) ) ;
#2174 = ORIENTED_EDGE ( 'NONE', *, *, #4072, .T. ) ;
#2175 = EDGE_CURVE ( 'NONE', #371, #5113, #5687, .T. ) ;
#2176 = ORIENTED_EDGE ( 'NONE', *, *, #4177, .T. ) ;
#2177 = EDGE_LOOP ( 'NONE', ( #874, #1823, #217, #3763 ) ) ;
#2178 = LINE ( 'NONE', #5161, #4292 ) ;
#2179 = ADVANCED_FACE ( 'NONE', ( #5131 ), #2136, .T. ) ;
#2180 = VECTOR ( 'NONE', #7427, 1000.000000000000000 ) ;
#2181 = CARTESIAN_POINT ( 'NONE',  ( 119.9981648402868899, 207.8429183184021269, 10.00000000000000178 ) ) ;
#2182 = DIRECTION ( 'NONE',  ( 1.000000000000000000, 0.000000000000000000, 0.000000000000000000 ) ) ;
#2183 = VERTEX_POINT ( 'NONE', #4503 ) ;
#2184 = VECTOR ( 'NONE', #5450, 1000.000000000000000 ) ;
#2185 = AXIS2_PLACEMENT_3D ( 'NONE', #2196, #7546, #2160 ) ;
#2186 = CARTESIAN_POINT ( 'NONE',  ( -20.63749999999999574, 4.592425496802574367E-15, 37.50000000000000000 ) ) ;
#2187 = CARTESIAN_POINT ( 'NONE',  ( 3.500000000000006661, 3.860699034312030436E-15, 31.52499999999999858 ) ) ;
#2188 = DIRECTION ( 'NONE',  ( 0.9845265360683707057, 0.1752355551171480841, 0.000000000000000000 ) ) ;
#2189 = AXIS2_PLACEMENT_3D ( 'NONE', #6607, #4561, #1197 ) ;
#2190 = CARTESIAN_POINT ( 'NONE',  ( 350.0000000000000000, 300.0000000000000000, -120.0000000000000000 ) ) ;
#2191 = ORIENTED_EDGE ( 'NONE', *, *, #4809, .T. ) ;
#2192 = CARTESIAN_POINT ( 'NONE',  ( -4.680456609903976606, -6.535341423375598424, -0.01688885742777120058 ) ) ;
#2193 = VECTOR ( 'NONE', #5322, 1000.000000000000000 ) ;
#2194 = CARTESIAN_POINT ( 'NONE',  ( 4.250000000000000000, 0.000000000000000000, -4.149444346342716194 ) ) ;
#2195 = CARTESIAN_POINT ( 'NONE',  ( -63.76644452187067458, 49.96174644486002592, 0.000000000000000000 ) ) ;
#2196 = CARTESIAN_POINT ( 'NONE',  ( 85.00000000000000000, 9.720002580593245511E-13, 10.00000000000000000 ) ) ;
#2197 = DIRECTION ( 'NONE',  ( -0.000000000000000000, -0.000000000000000000, 1.000000000000000000 ) ) ;
#2198 = ITEM_DEFINED_TRANSFORMATION ( 'NONE', 'NONE', #1451,  #7485 ) ;
#2199 = DIRECTION ( 'NONE',  ( -0.000000000000000000, -0.000000000000000000, 1.000000000000000000 ) ) ;
#2200 = AXIS2_PLACEMENT_3D ( 'NONE', #340, #1568, #4721 ) ;
#2201 = VERTEX_POINT ( 'NONE', #203 ) ;
#2202 = AXIS2_PLACEMENT_3D ( 'NONE', #6764, #2550, #4937 ) ;
#2203 = EDGE_LOOP ( 'NONE', ( #6601, #838, #1251, #717 ) ) ;
#2204 = ORIENTED_EDGE ( 'NONE', *, *, #3180, .F. ) ;
#2205 = DIRECTION ( 'NONE',  ( -0.000000000000000000, -0.000000000000000000, -1.000000000000000000 ) ) ;
#2206 = AXIS2_PLACEMENT_3D ( 'NONE', #4634, #1678, #7583 ) ;
#2207 = DIRECTION ( 'NONE',  ( 1.000000000000000000, 0.000000000000000000, 0.000000000000000000 ) ) ;
#2208 = AXIS2_PLACEMENT_3D ( 'NONE', #2239, #4630, #1634 ) ;
#2209 = EDGE_CURVE ( 'NONE', #7320, #7642, #3211, .T. ) ;
#2210 = CARTESIAN_POINT ( 'NONE',  ( 4.680456609903970389, 6.535341423375591319, -0.01688885742776586110 ) ) ;
#2211 = CARTESIAN_POINT ( 'NONE',  ( -39.64284999284934941, -144.6666666666667140, 5.000000000000000000 ) ) ;
#2212 = CARTESIAN_POINT ( 'NONE',  ( 0.000000000000000000, 0.000000000000000000, 0.000000000000000000 ) ) ;
#2213 = SURFACE_SIDE_STYLE ('',( #540 ) ) ;
#2214 = DIRECTION ( 'NONE',  ( 0.000000000000000000, 0.000000000000000000, 1.000000000000000000 ) ) ;
#2215 = ADVANCED_FACE ( 'NONE', ( #7425 ), #4980, .F. ) ;
#2216 = EDGE_CURVE ( 'NONE', #7160, #2888, #7407, .T. ) ;
#2217 = AXIS2_PLACEMENT_3D ( 'NONE', #4158, #2985, #6721 ) ;
#2218 = ORIENTED_EDGE ( 'NONE', *, *, #3985, .T. ) ;
#2219 = EDGE_CURVE ( 'NONE', #1026, #3054, #3617, .T. ) ;
#2220 = VERTEX_POINT ( 'NONE', #4542 ) ;
#2221 = ORIENTED_EDGE ( 'NONE', *, *, #6312, .F. ) ;
#2222 = FACE_OUTER_BOUND ( 'NONE', #4382, .T. ) ;
#2223 =( NAMED_UNIT ( * ) SI_UNIT ( $, .STERADIAN. ) SOLID_ANGLE_UNIT ( ) );
#2224 = EDGE_CURVE ( 'NONE', #545, #371, #6950, .T. ) ;
#2225 = AXIS2_PLACEMENT_3D ( 'NONE', #27, #2409, #3692 ) ;
#2226 = CARTESIAN_POINT ( 'NONE',  ( 0.000000000000000000, 0.000000000000000000, -112.9999999999999716 ) ) ;
#2227 = CARTESIAN_POINT ( 'NONE',  ( 0.6543471694412384965, 8.859816792613651515, -0.4964154566687972170 ) ) ;
#2228 = EDGE_LOOP ( 'NONE', ( #1080, #1012, #5527, #1071, #155, #5759 ) ) ;
#2229 = ORIENTED_EDGE ( 'NONE', *, *, #3702, .T. ) ;
#2230 = PLANE ( 'NONE',  #5632 ) ;
#2231 = CARTESIAN_POINT ( 'NONE',  ( 79.75000000000000000, 9.726431976288768917E-13, 10.00000000000000000 ) ) ;
#2232 = CARTESIAN_POINT ( 'NONE',  ( -63.76644452187068879, 49.96174644486002592, 24.17200000000001125 ) ) ;
#2233 = DIRECTION ( 'NONE',  ( 1.000000000000000000, 0.000000000000000000, 0.000000000000000000 ) ) ;
#2234 = ORIENTED_EDGE ( 'NONE', *, *, #463, .F. ) ;
#2235 = VERTEX_POINT ( 'NONE', #871 ) ;
#2236 = AXIS2_PLACEMENT_3D ( 'NONE', #3018, #1798, #720 ) ;
#2237 = DIRECTION ( 'NONE',  ( 1.000000000000000000, 0.000000000000000000, -0.000000000000000000 ) ) ;
#2238 = CARTESIAN_POINT ( 'NONE',  ( 0.000000000000000000, 0.000000000000000000, -139.9999999999999716 ) ) ;
#2239 = CARTESIAN_POINT ( 'NONE',  ( -20.63749999999999574, 0.000000000000000000, 0.000000000000000000 ) ) ;
#2240 = CARTESIAN_POINT ( 'NONE',  ( -64.59444452187068464, 49.96174644486002592, -65.00000000000000000 ) ) ;
#2241 = DIRECTION ( 'NONE',  ( 0.000000000000000000, 0.000000000000000000, -1.000000000000000000 ) ) ;
#2242 = AXIS2_PLACEMENT_3D ( 'NONE', #5289, #1584, #2849 ) ;
#2243 = CARTESIAN_POINT ( 'NONE',  ( -28.32536770618215982, 3.150165759062969695, 13.00000000000000178 ) ) ;
#2244 = EDGE_LOOP ( 'NONE', ( #431, #1190 ) ) ;
#2245 = VERTEX_POINT ( 'NONE', #6363 ) ;
#2246 = ORIENTED_EDGE ( 'NONE', *, *, #411, .T. ) ;
#2247 = CONICAL_SURFACE ( 'NONE', #3120, 37.49999999999997868, 1.029744258676654090 ) ;
#2248 = CARTESIAN_POINT ( 'NONE',  ( -8.000000000000000000, 4.618802153517003184, -0.7145311798163286321 ) ) ;
#2249 = DIRECTION ( 'NONE',  ( -0.000000000000000000, -0.000000000000000000, 1.000000000000000000 ) ) ;
#2250 = FACE_OUTER_BOUND ( 'NONE', #4663, .T. ) ;
#2251 = DIRECTION ( 'NONE',  ( 0.000000000000000000, 0.000000000000000000, 1.000000000000000000 ) ) ;
#2252 = CARTESIAN_POINT ( 'NONE',  ( 0.000000000000000000, 0.000000000000000000, 10.00000000000000000 ) ) ;
#2253 = DIRECTION ( 'NONE',  ( 1.000000000000000000, 0.000000000000000000, 0.000000000000000000 ) ) ;
#2254 = AXIS2_PLACEMENT_3D ( 'NONE', #3570, #3998, #5301 ) ;
#2255 = ORIENTED_EDGE ( 'NONE', *, *, #5817, .F. ) ;
#2256 = ORIENTED_EDGE ( 'NONE', *, *, #6553, .T. ) ;
#2257 = EDGE_LOOP ( 'NONE', ( #3728, #3351 ) ) ;
#2258 = CARTESIAN_POINT ( 'NONE',  ( -8.000000000000000000, 3.115336682267009660, -4.380606868608495574 ) ) ;
#2259 = EDGE_CURVE ( 'NONE', #7537, #3787, #1751, .T. ) ;
#2260 = CARTESIAN_POINT ( 'NONE',  ( -202.5929183184026954, 119.9981648402859378, -50.00000000000000000 ) ) ;
#2261 = AXIS2_PLACEMENT_3D ( 'NONE', #6691, #2485, #1927 ) ;
#2262 = DIRECTION ( 'NONE',  ( -0.000000000000000000, -0.000000000000000000, 1.000000000000000000 ) ) ;
#2263 = VERTEX_POINT ( 'NONE', #2893 ) ;
#2264 = EDGE_CURVE ( 'NONE', #4532, #4648, #7654, .T. ) ;
#2265 = AXIS2_PLACEMENT_3D ( 'NONE', #3317, #7568, #2105 ) ;
#2266 = DIRECTION ( 'NONE',  ( -1.000000000000000000, 0.000000000000000000, 0.000000000000000000 ) ) ;
#2267 = DIRECTION ( 'NONE',  ( -1.000000000000000000, 0.000000000000000000, 0.000000000000000000 ) ) ;
#2268 = CARTESIAN_POINT ( 'NONE',  ( 1.313474075707211641, 8.479269695850861766, -4.383279549040159928 ) ) ;
#2269 = DIRECTION ( 'NONE',  ( 1.000000000000000000, 0.000000000000000000, 0.000000000000000000 ) ) ;
#2270 = EDGE_LOOP ( 'NONE', ( #2712, #7610, #6037, #896 ) ) ;
#2271 = VECTOR ( 'NONE', #2292, 1000.000000000000000 ) ;
#2272 = ORIENTED_EDGE ( 'NONE', *, *, #5766, .T. ) ;
#2273 = CARTESIAN_POINT ( 'NONE',  ( -5.355005115540899752, -6.145890662064662280, -0.08224679563971788732 ) ) ;
#2274 = DIRECTION ( 'NONE',  ( 1.000000000000000000, 0.000000000000000000, 0.000000000000000000 ) ) ;
#2275 = PRESENTATION_LAYER_ASSIGNMENT (  '', '', ( #6178 ) ) ;
#2276 = CARTESIAN_POINT ( 'NONE',  ( 29.99999999999999289, 0.000000000000000000, -139.9999999999999716 ) ) ;
#2277 = LINE ( 'NONE', #2783, #4141 ) ;
#2278 = DIRECTION ( 'NONE',  ( 1.000000000000000000, 0.000000000000000000, 0.000000000000000000 ) ) ;
#2279 = EDGE_CURVE ( 'NONE', #5913, #2220, #6518, .T. ) ;
#2280 = ITEM_DEFINED_TRANSFORMATION ( 'NONE', 'NONE', #2481,  #7485 ) ;
#2281 = DIRECTION ( 'NONE',  ( 0.000000000000000000, 0.000000000000000000, 1.000000000000000000 ) ) ;
#2282 = ORIENTED_EDGE ( 'NONE', *, *, #5521, .T. ) ;
#2283 = VERTEX_POINT ( 'NONE', #1107 ) ;
#2284 = CIRCLE ( 'NONE', #5292, 28.50000000000000355 ) ;
#2285 = ORIENTED_EDGE ( 'NONE', *, *, #6258, .F. ) ;
#2286 = CARTESIAN_POINT ( 'NONE',  ( -4.681481898397000130, 6.534749472788145219, 4.804370876826391523E-15 ) ) ;
#2287 = DIRECTION ( 'NONE',  ( -0.000000000000000000, -0.000000000000000000, -1.000000000000000000 ) ) ;
#2288 = CARTESIAN_POINT ( 'NONE',  ( -20.63749999999999574, 0.000000000000000000, 0.000000000000000000 ) ) ;
#2289 = PRESENTATION_STYLE_ASSIGNMENT (( #339 ) ) ;
#2290 = CIRCLE ( 'NONE', #1790, 40.00000000000000000 ) ;
#2291 = DIRECTION ( 'NONE',  ( 1.000000000000000000, 0.000000000000000000, 0.000000000000000000 ) ) ;
#2292 = DIRECTION ( 'NONE',  ( -0.000000000000000000, -0.000000000000000000, 1.000000000000000000 ) ) ;
#2293 = ORIENTED_EDGE ( 'NONE', *, *, #601, .F. ) ;
#2294 = ORIENTED_EDGE ( 'NONE', *, *, #5817, .T. ) ;
#2295 = CIRCLE ( 'NONE', #515, 5.000000000000000888 ) ;
#2296 =( REPRESENTATION_RELATIONSHIP ('NONE','NONE', #1229, #5012 ) REPRESENTATION_RELATIONSHIP_WITH_TRANSFORMATION ( #5107 )SHAPE_REPRESENTATION_RELATIONSHIP( ) );
#2297 = ORIENTED_EDGE ( 'NONE', *, *, #4384, .F. ) ;
#2298 = DIRECTION ( 'NONE',  ( 0.000000000000000000, 0.000000000000000000, -1.000000000000000000 ) ) ;
#2299 = CARTESIAN_POINT ( 'NONE',  ( -68.76644452187068168, 49.96174644486002592, 10.00000000000000000 ) ) ;
#2300 =( NAMED_UNIT ( * ) SI_UNIT ( $, .STERADIAN. ) SOLID_ANGLE_UNIT ( ) );
#2301 = CARTESIAN_POINT ( 'NONE',  ( -105.4635834177243794, 106.6650485055563990, 0.000000000000000000 ) ) ;
#2302 = EDGE_CURVE ( 'NONE', #3642, #5742, #7106, .T. ) ;
#2303 = CARTESIAN_POINT ( 'NONE',  ( -29.99999999999999289, 3.673940397442058389E-15, -82.99999999999995737 ) ) ;
#2304 = ORIENTED_EDGE ( 'NONE', *, *, #5352, .T. ) ;
#2305 = ORIENTED_EDGE ( 'NONE', *, *, #4893, .T. ) ;
#2306 = SHAPE_REPRESENTATION ( 'circlip for shafts heavy_din_Circlip DIN 471 - 60 x 3', ( #7485 ), #6367 ) ;
#2307 = CARTESIAN_POINT ( 'NONE',  ( -202.5929183184021269, 119.9981648402869467, 10.00000000000000178 ) ) ;
#2308 = CARTESIAN_POINT ( 'NONE',  ( -68.76644452187068168, 49.96174644486002592, 0.000000000000000000 ) ) ;
#2309 = ADVANCED_FACE ( 'NONE', ( #6475 ), #1754, .T. ) ;
#2310 = LINE ( 'NONE', #7146, #3009 ) ;
#2311 = CARTESIAN_POINT ( 'NONE',  ( -20.63749999999999929, 3.860699034312030436E-15, 31.52499999999999858 ) ) ;
#2312 = EDGE_CURVE ( 'NONE', #5752, #1868, #5580, .T. ) ;
#2313 = ORIENTED_EDGE ( 'NONE', *, *, #5477, .F. ) ;
#2314 = EDGE_CURVE ( 'NONE', #3873, #7291, #1490, .T. ) ;
#2315 = ORIENTED_EDGE ( 'NONE', *, *, #3741, .F. ) ;
#2316 = EDGE_CURVE ( 'NONE', #520, #1212, #2385, .T. ) ;
#2317 = CARTESIAN_POINT ( 'NONE',  ( 0.000000000000000000, 0.000000000000000000, 10.00000000000000888 ) ) ;
#2318 = LINE ( 'NONE', #6410, #2488 ) ;
#2319 = VECTOR ( 'NONE', #5125, 1000.000000000000000 ) ;
#2320 = CARTESIAN_POINT ( 'NONE',  ( 8.000000000000000000, 0.7809653281576046657, 3.049318610115479988E-17 ) ) ;
#2321 = CARTESIAN_POINT ( 'NONE',  ( -68.76644452187068168, 49.96174644486002592, -65.00000000000000000 ) ) ;
#2322 = CYLINDRICAL_SURFACE ( 'NONE', #361, 30.00000000000000000 ) ;
#2323 = CARTESIAN_POINT ( 'NONE',  ( 3.499999999999996003, 0.000000000000000000, 0.000000000000000000 ) ) ;
#2324 = EDGE_CURVE ( 'NONE', #5401, #6223, #3520, .T. ) ;
#2325 = LINE ( 'NONE', #5778, #4840 ) ;
#2326 = ORIENTED_EDGE ( 'NONE', *, *, #84, .T. ) ;
#2327 = ORIENTED_EDGE ( 'NONE', *, *, #2216, .F. ) ;
#2328 = CIRCLE ( 'NONE', #4195, 199.9963296805737230 ) ;
#2329 = VERTEX_POINT ( 'NONE', #1587 ) ;
#2330 = EDGE_CURVE ( 'NONE', #1561, #2827, #390, .T. ) ;
#2331 = DIRECTION ( 'NONE',  ( -5.635681009894454322E-17, -1.505185443864239327E-19, -1.000000000000000000 ) ) ;
#2332 = DIRECTION ( 'NONE',  ( 1.000000000000000000, 0.000000000000000000, 0.000000000000000000 ) ) ;
#2333 = DIRECTION ( 'NONE',  ( -1.000000000000000000, 0.000000000000000000, 0.000000000000000000 ) ) ;
#2334 = DIRECTION ( 'NONE',  ( 0.000000000000000000, 0.000000000000000000, 1.000000000000000000 ) ) ;
#2335 = FILL_AREA_STYLE_COLOUR ( '', #50 ) ;
#2336 = CARTESIAN_POINT ( 'NONE',  ( 7.345652830558762503, -4.996589667937383794, -0.4964154566687976611 ) ) ;
#2337 = ORIENTED_EDGE ( 'NONE', *, *, #4723, .T. ) ;
#2338 = ORIENTED_EDGE ( 'NONE', *, *, #1240, .F. ) ;
#2339 = VECTOR ( 'NONE', #835, 1000.000000000000000 ) ;
#2340 = ORIENTED_EDGE ( 'NONE', *, *, #1003, .F. ) ;
#2341 = LINE ( 'NONE', #6431, #5297 ) ;
#2342 = DIRECTION ( 'NONE',  ( 1.000000000000000000, 0.000000000000000000, 0.000000000000000000 ) ) ;
#2343 =( LENGTH_UNIT ( ) NAMED_UNIT ( * ) SI_UNIT ( .MILLI., .METRE. ) );
#2344 = CYLINDRICAL_SURFACE ( 'NONE', #7596, 30.00000000000000000 ) ;
#2345 = ORIENTED_EDGE ( 'NONE', *, *, #4700, .T. ) ;
#2346 = DIRECTION ( 'NONE',  ( 1.000000000000000000, 0.000000000000000000, 0.000000000000000000 ) ) ;
#2347 = CARTESIAN_POINT ( 'NONE',  ( -37.49999999999997868, 0.000000000000000000, -112.9999999999999716 ) ) ;
#2348 = DIRECTION ( 'NONE',  ( -0.4999999999999918954, -0.8660254037844432595, 0.000000000000000000 ) ) ;
#2349 = DIRECTION ( 'NONE',  ( 0.000000000000000000, 0.000000000000000000, 1.000000000000000000 ) ) ;
#2350 = EDGE_LOOP ( 'NONE', ( #70, #4932 ) ) ;
#2351 = ORIENTED_EDGE ( 'NONE', *, *, #6649, .T. ) ;
#2352 = ADVANCED_FACE ( 'NONE', ( #3989 ), #2773, .F. ) ;
#2353 = ORIENTED_EDGE ( 'NONE', *, *, #3219, .T. ) ;
#2354 = CIRCLE ( 'NONE', #7131, 4.171999999999995268 ) ;
#2355 = CARTESIAN_POINT ( 'NONE',  ( -3.200000000000007727, 3.710679801416480038E-15, 30.30000000000000071 ) ) ;
#2356 = CARTESIAN_POINT ( 'NONE',  ( 0.000000000000000000, 0.000000000000000000, 0.000000000000000000 ) ) ;
#2357 = EDGE_CURVE ( 'NONE', #952, #5940, #6912, .T. ) ;
#2358 = EDGE_CURVE ( 'NONE', #4116, #4257, #3138, .T. ) ;
#2359 = CARTESIAN_POINT ( 'NONE',  ( 8.000000000000000000, 4.618802153517013842, -0.7145311798163319628 ) ) ;
#2360 = CARTESIAN_POINT ( 'NONE',  ( -68.76644452187068168, 49.96174644486002592, 0.000000000000000000 ) ) ;
#2361 = CARTESIAN_POINT ( 'NONE',  ( 0.000000000000000000, 0.000000000000000000, -79.99999999999995737 ) ) ;
#2362 = EDGE_CURVE ( 'NONE', #5007, #5051, #5898, .T. ) ;
#2363 = CARTESIAN_POINT ( 'NONE',  ( 0.5700000000000001732, -28.49429942988597020, -3.000000000000000000 ) ) ;
#2364 = PRODUCT_DEFINITION_CONTEXT ( 'detailed design', #5505, 'design' ) ;
#2365 = ORIENTED_EDGE ( 'NONE', *, *, #5920, .T. ) ;
#2366 = ORIENTED_EDGE ( 'NONE', *, *, #5394, .T. ) ;
#2367 = CARTESIAN_POINT ( 'NONE',  ( 3.200000000000007727, 0.000000000000000000, 0.000000000000000000 ) ) ;
#2368 = EDGE_CURVE ( 'NONE', #6897, #47, #105, .T. ) ;
#2369 = AXIS2_PLACEMENT_3D ( 'NONE', #4392, #3808, #5619 ) ;
#2370 = DIRECTION ( 'NONE',  ( 0.000000000000000000, 0.000000000000000000, -1.000000000000000000 ) ) ;
#2371 = CARTESIAN_POINT ( 'NONE',  ( -29.99999999999999289, 3.673940397442058389E-15, -139.9999999999999716 ) ) ;
#2372 = DIRECTION ( 'NONE',  ( 0.9938725510941111008, -0.1105321318969464395, 0.000000000000000000 ) ) ;
#2373 = FACE_OUTER_BOUND ( 'NONE', #2769, .T. ) ;
#2374 = DIRECTION ( 'NONE',  ( -0.000000000000000000, -0.000000000000000000, -1.000000000000000000 ) ) ;
#2375 = ORIENTED_EDGE ( 'NONE', *, *, #4853, .T. ) ;
#2376 = AXIS2_PLACEMENT_3D ( 'NONE', #619, #4913, #4280 ) ;
#2377 = EDGE_LOOP ( 'NONE', ( #6050, #3200, #4210, #6603 ) ) ;
#2378 = ORIENTED_EDGE ( 'NONE', *, *, #3700, .T. ) ;
#2379 = LINE ( 'NONE', #1057, #5169 ) ;
#2380 = CARTESIAN_POINT ( 'NONE',  ( -68.76644452187068168, 49.96174644486002592, 24.17200000000001125 ) ) ;
#2381 = CIRCLE ( 'NONE', #3250, 37.50000000000000000 ) ;
#2382 = CYLINDRICAL_SURFACE ( 'NONE', #2817, 279.9963296805736945 ) ;
#2383 = VERTEX_POINT ( 'NONE', #5805 ) ;
#2384 = ORIENTED_EDGE ( 'NONE', *, *, #3920, .F. ) ;
#2385 = CIRCLE ( 'NONE', #856, 4.999999999999990230 ) ;
#2386 = CARTESIAN_POINT ( 'NONE',  ( 10.00000000000000000, 42.00000000000000000, 0.000000000000000000 ) ) ;
#2387 = CIRCLE ( 'NONE', #5269, 35.25000000000000000 ) ;
#2388 = CARTESIAN_POINT ( 'NONE',  ( -10.00000000000000000, 28.28427124746189136, -139.9999999999999716 ) ) ;
#2389 = VECTOR ( 'NONE', #6198, 1000.000000000000000 ) ;
#2390 = DIRECTION ( 'NONE',  ( 1.000000000000000000, 0.000000000000000000, 0.000000000000000000 ) ) ;
#2391 = EDGE_LOOP ( 'NONE', ( #3265, #6337, #7699, #7108, #752, #7670 ) ) ;
#2392 = ORIENTED_EDGE ( 'NONE', *, *, #7691, .T. ) ;
#2393 = CIRCLE ( 'NONE', #2004, 32.25000000000000000 ) ;
#2394 = ORIENTED_EDGE ( 'NONE', *, *, #5334, .T. ) ;
#2395 = DIRECTION ( 'NONE',  ( -1.000000000000000000, 0.000000000000000000, 0.000000000000000000 ) ) ;
#2396 = FACE_BOUND ( 'NONE', #3451, .T. ) ;
#2397 = LINE ( 'NONE', #3681, #3896 ) ;
#2398 = CARTESIAN_POINT ( 'NONE',  ( -5.554394503829287011, 27.95350964898380752, -79.99999999999995737 ) ) ;
#2399 = CARTESIAN_POINT ( 'NONE',  ( -64.59444452187068464, 49.96174644486002592, 25.00000000000000000 ) ) ;
#2400 = EDGE_CURVE ( 'NONE', #5402, #1121, #2310, .T. ) ;
#2401 = ORIENTED_EDGE ( 'NONE', *, *, #7219, .F. ) ;
#2402 =( REPRESENTATION_RELATIONSHIP ('NONE','NONE', #1229, #1433 ) REPRESENTATION_RELATIONSHIP_WITH_TRANSFORMATION ( #2436 )SHAPE_REPRESENTATION_RELATIONSHIP( ) );
#2403 = ORIENTED_EDGE ( 'NONE', *, *, #6890, .F. ) ;
#2404 = CIRCLE ( 'NONE', #3275, 279.9963296805736945 ) ;
#2405 = EDGE_CURVE ( 'NONE', #3290, #1651, #4132, .T. ) ;
#2406 = DIRECTION ( 'NONE',  ( 1.000000000000000000, 0.000000000000000000, 0.000000000000000000 ) ) ;
#2407 = DIRECTION ( 'NONE',  ( -1.000000000000000000, 0.000000000000000000, 0.000000000000000000 ) ) ;
#2408 = DIRECTION ( 'NONE',  ( -0.000000000000000000, -0.000000000000000000, -1.000000000000000000 ) ) ;
#2409 = DIRECTION ( 'NONE',  ( -5.551115123125782702E-17, 0.000000000000000000, -1.000000000000000000 ) ) ;
#2410 = DIRECTION ( 'NONE',  ( 0.000000000000000000, 0.000000000000000000, 1.000000000000000000 ) ) ;
#2411 = DIRECTION ( 'NONE',  ( 0.9412010056177179118, 0.3378471059875997051, 1.703375277368107492E-17 ) ) ;
#2412 = EDGE_CURVE ( 'NONE', #256, #5216, #4637, .T. ) ;
#2413 = VERTEX_POINT ( 'NONE', #4581 ) ;
#2414 = ORIENTED_EDGE ( 'NONE', *, *, #4941, .T. ) ;
#2415 = EDGE_CURVE ( 'NONE', #2235, #5791, #3401, .T. ) ;
#2416 = ORIENTED_EDGE ( 'NONE', *, *, #754, .T. ) ;
#2417 = CIRCLE ( 'NONE', #636, 29.99999999999999289 ) ;
#2418 = CARTESIAN_POINT ( 'NONE',  ( -3.500000000000006661, 0.000000000000000000, 0.000000000000000000 ) ) ;
#2419 = SURFACE_STYLE_USAGE ( .BOTH. , #2 ) ;
#2420 = SHAPE_REPRESENTATION_RELATIONSHIP ( 'NONE' , 'NONE' ,  #5012, #4435 ) ;
#2421 = DIRECTION ( 'NONE',  ( 0.000000000000000000, 0.000000000000000000, -1.000000000000000000 ) ) ;
#2422 = ADVANCED_FACE ( 'NONE', ( #715 ), #6006, .T. ) ;
#2423 = VERTEX_POINT ( 'NONE', #2428 ) ;
#2424 = ORIENTED_EDGE ( 'NONE', *, *, #4511, .T. ) ;
#2425 = AXIS2_PLACEMENT_3D ( 'NONE', #3536, #1643, #1683 ) ;
#2426 = ADVANCED_FACE ( 'NONE', ( #639 ), #1831, .F. ) ;
#2427 = DIRECTION ( 'NONE',  ( 1.000000000000000000, 0.000000000000000000, 0.000000000000000000 ) ) ;
#2428 = CARTESIAN_POINT ( 'NONE',  ( 1.677050983124841466, 4.316879966994421072E-15, -35.25000000000000000 ) ) ;
#2429 = DIRECTION ( 'NONE',  ( -0.000000000000000000, -0.000000000000000000, 1.000000000000000000 ) ) ;
#2430 = VERTEX_POINT ( 'NONE', #3012 ) ;
#2431 = ORIENTED_EDGE ( 'NONE', *, *, #4223, .F. ) ;
#2432 = CARTESIAN_POINT ( 'NONE',  ( 350.0000000000000000, 37.15382499588017140, -82.99999999999998579 ) ) ;
#2433 = CARTESIAN_POINT ( 'NONE',  ( -3.499999999999996003, 4.405666859932603897E-15, 35.97500000000000142 ) ) ;
#2434 = DIRECTION ( 'NONE',  ( -0.000000000000000000, -0.000000000000000000, -1.000000000000000000 ) ) ;
#2435 = LINE ( 'NONE', #7352, #724 ) ;
#2436 = ITEM_DEFINED_TRANSFORMATION ( 'NONE', 'NONE', #822,  #7485 ) ;
#2437 = AXIS2_PLACEMENT_3D ( 'NONE', #3325, #5727, #2117 ) ;
#2438 = LINE ( 'NONE', #7240, #7211 ) ;
#2439 = ORIENTED_EDGE ( 'NONE', *, *, #3702, .F. ) ;
#2440 = VECTOR ( 'NONE', #866, 1000.000000000000000 ) ;
#2441 = PRODUCT_DEFINITION_FORMATION_WITH_SPECIFIED_SOURCE ( 'ANY', '', #5672, .NOT_KNOWN. ) ;
#2442 = CARTESIAN_POINT ( 'NONE',  ( -68.76644452187068168, 49.96174644486002592, 25.00000000000000000 ) ) ;
#2443 = CARTESIAN_POINT ( 'NONE',  ( 1.677050983124841466, 0.000000000000000000, 0.000000000000000000 ) ) ;
#2444 = CARTESIAN_POINT ( 'NONE',  ( -119.9981648402868046, 207.8429183184021554, 10.00000000000000000 ) ) ;
#2445 = CARTESIAN_POINT ( 'NONE',  ( -207.8429183184026954, 119.9981648402859946, -124.7000000000000028 ) ) ;
#2446 = APPLICATION_CONTEXT ( 'automotive_design' ) ;
#2447 = CARTESIAN_POINT ( 'NONE',  ( 1.499999999999999334, -33.63777638310832430, -3.000000000000000000 ) ) ;
#2448 = DIRECTION ( 'NONE',  ( -2.485795968188197231E-17, 1.883273162252411239E-17, 1.000000000000000000 ) ) ;
#2449 = CIRCLE ( 'NONE', #6594, 10.00000000000000178 ) ;
#2450 = DIRECTION ( 'NONE',  ( -0.7071067811865504593, 0.000000000000000000, -0.7071067811865445751 ) ) ;
#2451 = EDGE_LOOP ( 'NONE', ( #4442, #7521, #3780, #6080 ) ) ;
#2452 = ORIENTED_EDGE ( 'NONE', *, *, #6406, .F. ) ;
#2453 = EDGE_CURVE ( 'NONE', #3350, #6223, #1341, .T. ) ;
#2454 = EDGE_LOOP ( 'NONE', ( #1141, #6828, #1750, #4646, #923, #1011 ) ) ;
#2455 = AXIS2_PLACEMENT_3D ( 'NONE', #4054, #5878, #4178 ) ;
#2456 = CARTESIAN_POINT ( 'NONE',  ( 11.50644898236017433, -35.69105814929478981, -3.000000000000000000 ) ) ;
#2457 = CARTESIAN_POINT ( 'NONE',  ( 5.249999999999474198, 239.9963296805737230, -120.0000000000000000 ) ) ;
#2458 = ADVANCED_FACE ( 'NONE', ( #1793 ), #4814, .F. ) ;
#2459 = EDGE_CURVE ( 'NONE', #6736, #4191, #44, .T. ) ;
#2460 = CARTESIAN_POINT ( 'NONE',  ( -213.0929183184026670, 119.9981648402859378, -120.0000000000000000 ) ) ;
#2461 = EDGE_CURVE ( 'NONE', #1532, #2556, #2470, .T. ) ;
#2462 = AXIS2_PLACEMENT_3D ( 'NONE', #3274, #6975, #5076 ) ;
#2463 = EDGE_LOOP ( 'NONE', ( #3605, #4352, #6627, #3263 ) ) ;
#2464 = AXIS2_PLACEMENT_3D ( 'NONE', #2732, #389, #5053 ) ;
#2465 = EDGE_LOOP ( 'NONE', ( #2760, #4362, #6266, #2907, #22, #2204, #3465, #6818 ) ) ;
#2466 = ADVANCED_FACE ( 'NONE', ( #5525 ), #5400, .T. ) ;
#2467 = DIRECTION ( 'NONE',  ( -0.000000000000000000, -0.000000000000000000, 1.000000000000000000 ) ) ;
#2468 = AXIS2_PLACEMENT_3D ( 'NONE', #6852, #1438, #7078 ) ;
#2469 = MECHANICAL_DESIGN_GEOMETRIC_PRESENTATION_REPRESENTATION (  '', ( #180 ), #5983 ) ;
#2470 = LINE ( 'NONE', #3638, #227 ) ;
#2471 = DIRECTION ( 'NONE',  ( 0.000000000000000000, 1.000000000000000000, -1.224646799147353207E-16 ) ) ;
#2472 = ORIENTED_EDGE ( 'NONE', *, *, #3571, .F. ) ;
#2473 = VECTOR ( 'NONE', #687, 1000.000000000000000 ) ;
#2474 = VERTEX_POINT ( 'NONE', #4777 ) ;
#2475 = PRODUCT_DEFINITION_SHAPE ( 'NONE', 'NONE',  #7793 ) ;
#2476 = DIRECTION ( 'NONE',  ( -0.000000000000000000, 0.000000000000000000, -1.000000000000000000 ) ) ;
#2477 = CARTESIAN_POINT ( 'NONE',  ( 207.8429183184020985, 119.9981648402868331, 10.00000000000000178 ) ) ;
#2478 = DIRECTION ( 'NONE',  ( 0.000000000000000000, 0.000000000000000000, 1.000000000000000000 ) ) ;
#2479 = DIRECTION ( 'NONE',  ( 1.000000000000000000, 0.000000000000000000, 0.000000000000000000 ) ) ;
#2480 = ITEM_DEFINED_TRANSFORMATION ( 'NONE', 'NONE', #4598,  #7485 ) ;
#2481 = AXIS2_PLACEMENT_3D ( 'NONE', #5905, #498, #5312 ) ;
#2482 = CARTESIAN_POINT ( 'NONE',  ( 5.459126460941064352, -34.89491303563345070, -3.000000000000000000 ) ) ;
#2483 = ORIENTED_EDGE ( 'NONE', *, *, #6829, .F. ) ;
#2484 = PLANE ( 'NONE',  #5951 ) ;
#2485 = DIRECTION ( 'NONE',  ( 1.000000000000000000, 0.000000000000000000, 0.000000000000000000 ) ) ;
#2486 = DIRECTION ( 'NONE',  ( 0.000000000000000000, 0.000000000000000000, -1.000000000000000000 ) ) ;
#2487 = DIRECTION ( 'NONE',  ( 0.000000000000000000, 0.000000000000000000, 1.000000000000000000 ) ) ;
#2488 = VECTOR ( 'NONE', #7113, 1000.000000000000000 ) ;
#2489 = CARTESIAN_POINT ( 'NONE',  ( -129.9038105676655164, -75.00000000000063949, 0.000000000000000000 ) ) ;
#2490 = LINE ( 'NONE', #734, #2950 ) ;
#2491 = VERTEX_POINT ( 'NONE', #5487 ) ;
#2492 = ORIENTED_EDGE ( 'NONE', *, *, #558, .F. ) ;
#2493 = CIRCLE ( 'NONE', #6891, 5.249999999999976907 ) ;
#2494 = ORIENTED_EDGE ( 'NONE', *, *, #4029, .F. ) ;
#2495 = CARTESIAN_POINT ( 'NONE',  ( -5.459126460941067016, -34.89491303563345070, -3.000000000000000000 ) ) ;
#2496 = LINE ( 'NONE', #7336, #7474 ) ;
#2497 = VECTOR ( 'NONE', #4086, 1000.000000000000000 ) ;
#2498 = ORIENTED_EDGE ( 'NONE', *, *, #2501, .F. ) ;
#2499 = EDGE_LOOP ( 'NONE', ( #1000, #2624, #6856, #3389 ) ) ;
#2500 = AXIS2_PLACEMENT_3D ( 'NONE', #455, #101, #6727 ) ;
#2501 = EDGE_CURVE ( 'NONE', #980, #1722, #7372, .T. ) ;
#2502 = FACE_OUTER_BOUND ( 'NONE', #4802, .T. ) ;
#2503 = CARTESIAN_POINT ( 'NONE',  ( 8.000000000000000000, 4.618802153517013842, -0.7145311798163319628 ) ) ;
#2504 = LINE ( 'NONE', #518, #4314 ) ;
#2505 = ORIENTED_EDGE ( 'NONE', *, *, #7355, .T. ) ;
#2506 = VECTOR ( 'NONE', #1545, 1000.000000000000000 ) ;
#2507 = EDGE_CURVE ( 'NONE', #6664, #688, #85, .T. ) ;
#2508 = ORIENTED_EDGE ( 'NONE', *, *, #6346, .T. ) ;
#2509 = DIRECTION ( 'NONE',  ( 1.000000000000000000, 0.000000000000000000, 0.000000000000000000 ) ) ;
#2510 = DIRECTION ( 'NONE',  ( -1.000000000000000000, 0.000000000000000000, 0.000000000000000000 ) ) ;
#2511 = VECTOR ( 'NONE', #5449, 1000.000000000000000 ) ;
#2512 = DIRECTION ( 'NONE',  ( 1.000000000000000000, 0.000000000000000000, 0.000000000000000000 ) ) ;
#2513 = LINE ( 'NONE', #1235, #7025 ) ;
#2514 = UNCERTAINTY_MEASURE_WITH_UNIT (LENGTH_MEASURE( 1.000000000000000082E-05 ), #4283, 'distance_accuracy_value', 'NONE');
#2515 = DIRECTION ( 'NONE',  ( -0.000000000000000000, -0.000000000000000000, 1.000000000000000000 ) ) ;
#2516 = EDGE_LOOP ( 'NONE', ( #1680, #6600, #2351, #7054 ) ) ;
#2517 = CIRCLE ( 'NONE', #2139, 5.249999999999976907 ) ;
#2518 = CARTESIAN_POINT ( 'NONE',  ( -199.9963296805737230, 2.449248649845333917E-14, -50.00000000000004263 ) ) ;
#2519 = ADVANCED_FACE ( 'NONE', ( #6083 ), #597, .T. ) ;
#2520 = CIRCLE ( 'NONE', #3394, 10.00000000000000178 ) ;
#2521 = CARTESIAN_POINT ( 'NONE',  ( 207.8429183184021269, 119.9981648402868331, -120.0000000000000000 ) ) ;
#2522 = CARTESIAN_POINT ( 'NONE',  ( -35.00000000000000711, 0.000000000000000000, -50.00000000000000000 ) ) ;
#2523 = DIRECTION ( 'NONE',  ( 0.5877852522924830181, -0.8090169943749402348, 0.000000000000000000 ) ) ;
#2524 = DIRECTION ( 'NONE',  ( 0.000000000000000000, 0.000000000000000000, -1.000000000000000000 ) ) ;
#2525 = DIRECTION ( 'NONE',  ( 0.000000000000000000, 0.000000000000000000, 1.000000000000000000 ) ) ;
#2526 = ORIENTED_EDGE ( 'NONE', *, *, #3708, .F. ) ;
#2527 = AXIS2_PLACEMENT_3D ( 'NONE', #5547, #2564, #7365 ) ;
#2528 = ORIENTED_EDGE ( 'NONE', *, *, #280, .F. ) ;
#2529 = VERTEX_POINT ( 'NONE', #2503 ) ;
#2530 = PLANE ( 'NONE',  #4798 ) ;
#2531 = FILL_AREA_STYLE_COLOUR ( '', #4023 ) ;
#2532 = AXIS2_PLACEMENT_3D ( 'NONE', #7104, #5966, #6004 ) ;
#2533 = DIRECTION ( 'NONE',  ( 1.000000000000000000, 0.000000000000000000, 0.000000000000000000 ) ) ;
#2534 = ORIENTED_EDGE ( 'NONE', *, *, #4723, .F. ) ;
#2535 = PRODUCT_DEFINITION_SHAPE ( 'NONE', 'NONE',  #7767 ) ;
#2536 = VERTEX_POINT ( 'NONE', #7305 ) ;
#2537 = VERTEX_POINT ( 'NONE', #1903 ) ;
#2538 = CIRCLE ( 'NONE', #7559, 31.52499999999999858 ) ;
#2539 = EDGE_CURVE ( 'NONE', #1983, #406, #606, .T. ) ;
#2540 = CARTESIAN_POINT ( 'NONE',  ( 35.00000000000000711, 4.286263797015737285E-15, -50.00000000000000000 ) ) ;
#2541 = DIRECTION ( 'NONE',  ( -0.000000000000000000, -0.000000000000000000, 1.000000000000000000 ) ) ;
#2542 = FACE_OUTER_BOUND ( 'NONE', #1906, .T. ) ;
#2543 = CONICAL_SURFACE ( 'NONE', #2163, 8.000000000000000000, 1.047197551196596299 ) ;
#2544 = FACE_OUTER_BOUND ( 'NONE', #1161, .T. ) ;
#2545 = ORIENTED_EDGE ( 'NONE', *, *, #4371, .F. ) ;
#2546 = ORIENTED_EDGE ( 'NONE', *, *, #1583, .F. ) ;
#2547 = APPLICATION_CONTEXT ( 'automotive_design' ) ;
#2548 = EDGE_CURVE ( 'NONE', #7134, #3827, #6046, .T. ) ;
#2549 = DIRECTION ( 'NONE',  ( 0.1303874742813643239, 0.9914631140645255858, 0.000000000000000000 ) ) ;
#2550 = DIRECTION ( 'NONE',  ( -1.000000000000000000, -0.000000000000000000, -0.000000000000000000 ) ) ;
#2551 = CARTESIAN_POINT ( 'NONE',  ( 3.499999999999996003, 37.19999999999999574, 0.000000000000000000 ) ) ;
#2552 = DIRECTION ( 'NONE',  ( 0.000000000000000000, 0.000000000000000000, -1.000000000000000000 ) ) ;
#2553 = EDGE_CURVE ( 'NONE', #746, #4490, #2626, .T. ) ;
#2554 = ADVANCED_FACE ( 'NONE', ( #2542 ), #3635, .T. ) ;
#2555 = CARTESIAN_POINT ( 'NONE',  ( 3.199999999999994404, 0.000000000000000000, 0.000000000000000000 ) ) ;
#2556 = VERTEX_POINT ( 'NONE', #3169 ) ;
#2557 = ADVANCED_FACE ( 'NONE', ( #2615 ), #3203, .T. ) ;
#2558 = CARTESIAN_POINT ( 'NONE',  ( -63.76644452187068879, 49.96174644486002592, 24.17200000000001125 ) ) ;
#2559 = VECTOR ( 'NONE', #1879, 1000.000000000000000 ) ;
#2560 = ADVANCED_FACE ( 'NONE', ( #5607 ), #1875, .T. ) ;
#2561 = SHAPE_REPRESENTATION ( 'Drive Shaft Keyed Hub', ( #7485 ), #7737 ) ;
#2562 = CARTESIAN_POINT ( 'NONE',  ( 8.000000000000000000, 0.000000000000000000, -4.700000000000000178 ) ) ;
#2563 = CARTESIAN_POINT ( 'NONE',  ( 213.0929183184021269, 119.9981648402868331, -50.00000000000000000 ) ) ;
#2564 = DIRECTION ( 'NONE',  ( -0.000000000000000000, -0.000000000000000000, 1.000000000000000000 ) ) ;
#2565 = LINE ( 'NONE', #657, #6215 ) ;
#2566 = ORIENTED_EDGE ( 'NONE', *, *, #794, .F. ) ;
#2567 = VECTOR ( 'NONE', #1501, 1000.000000000000000 ) ;
#2568 = EDGE_CURVE ( 'NONE', #2609, #5437, #3458, .T. ) ;
#2569 = EDGE_LOOP ( 'NONE', ( #6928, #1769, #1804, #3902 ) ) ;
#2570 = EDGE_LOOP ( 'NONE', ( #7367, #3818, #1214 ) ) ;
#2571 = DIRECTION ( 'NONE',  ( -0.000000000000000000, -0.000000000000000000, -1.000000000000000000 ) ) ;
#2572 = SURFACE_STYLE_USAGE ( .BOTH. , #4253 ) ;
#2573 = DIRECTION ( 'NONE',  ( 1.000000000000000000, 0.000000000000000000, 0.000000000000000000 ) ) ;
#2574 = EDGE_LOOP ( 'NONE', ( #7203, #5831 ) ) ;
#2575 = EDGE_LOOP ( 'NONE', ( #1667, #7727, #5992, #418 ) ) ;
#2576 = ORIENTED_EDGE ( 'NONE', *, *, #5572, .F. ) ;
#2577 = CIRCLE ( 'NONE', #164, 150.0000000000000568 ) ;
#2578 = CYLINDRICAL_SURFACE ( 'NONE', #1641, 5.249999999999976907 ) ;
#2579 = DIRECTION ( 'NONE',  ( -0.000000000000000000, -0.000000000000000000, -1.000000000000000000 ) ) ;
#2580 = AXIS2_PLACEMENT_3D ( 'NONE', #52, #167, #5456 ) ;
#2581 = CARTESIAN_POINT ( 'NONE',  ( 8.000000000000001776, -3.098204225878173457, -4.384209322808125364 ) ) ;
#2582 = VERTEX_POINT ( 'NONE', #3422 ) ;
#2583 = DIRECTION ( 'NONE',  ( 1.000000000000000000, 0.000000000000000000, 0.000000000000000000 ) ) ;
#2584 = CARTESIAN_POINT ( 'NONE',  ( 3.500000000000008438, 30.30000000000000071, 0.000000000000000000 ) ) ;
#2585 = CONTEXT_DEPENDENT_SHAPE_REPRESENTATION ( #1743, #4915 ) ;
#2586 = CARTESIAN_POINT ( 'NONE',  ( -74.01644452187024115, -49.96174644486060856, 10.00000000000000000 ) ) ;
#2587 = VECTOR ( 'NONE', #2410, 1000.000000000000000 ) ;
#2588 = ORIENTED_EDGE ( 'NONE', *, *, #218, .T. ) ;
#2589 = AXIS2_PLACEMENT_3D ( 'NONE', #4046, #7558, #7087 ) ;
#2590 = EDGE_CURVE ( 'NONE', #3533, #5822, #7418, .T. ) ;
#2591 = CARTESIAN_POINT ( 'NONE',  ( -5.134781488891348999E-13, 239.9963296805737230, -50.00000000000000000 ) ) ;
#2592 = EDGE_CURVE ( 'NONE', #7016, #4741, #2758, .T. ) ;
#2593 = CARTESIAN_POINT ( 'NONE',  ( -350.0000000000000000, 37.15382499588017140, -120.0000000000000000 ) ) ;
#2594 = AXIS2_PLACEMENT_3D ( 'NONE', #5748, #2798, #7050 ) ;
#2595 = ADVANCED_FACE ( 'NONE', ( #4607 ), #4645, .F. ) ;
#2596 = DIRECTION ( 'NONE',  ( 1.000000000000000000, 0.000000000000000000, 0.000000000000000000 ) ) ;
#2597 = CARTESIAN_POINT ( 'NONE',  ( 3.911624228440930828, 29.74389342193577690, 10.00000000000000000 ) ) ;
#2598 = DIRECTION ( 'NONE',  ( -7.358275397094339982E-17, -8.771527099359223764E-17, 0.9999999999999998890 ) ) ;
#2599 = PRODUCT_DEFINITION_SHAPE ( 'NONE', 'NONE',  #7783 ) ;
#2600 = SURFACE_SIDE_STYLE ('',( #6927 ) ) ;
#2601 = DIRECTION ( 'NONE',  ( 0.000000000000000000, 0.000000000000000000, 1.000000000000000000 ) ) ;
#2602 = ORIENTED_EDGE ( 'NONE', *, *, #5971, .F. ) ;
#2603 = ORIENTED_EDGE ( 'NONE', *, *, #4568, .F. ) ;
#2604 = VERTEX_POINT ( 'NONE', #4380 ) ;
#2605 = EDGE_CURVE ( 'NONE', #6450, #4002, #3871, .T. ) ;
#2606 = ORIENTED_EDGE ( 'NONE', *, *, #3920, .T. ) ;
#2607 = CARTESIAN_POINT ( 'NONE',  ( 32.49999999999997158, 3.980102097228894682E-15, -109.9956969048621716 ) ) ;
#2608 = DIRECTION ( 'NONE',  ( 0.000000000000000000, -0.000000000000000000, -1.000000000000000000 ) ) ;
#2609 = VERTEX_POINT ( 'NONE', #7052 ) ;
#2610 = VECTOR ( 'NONE', #3363, 1000.000000000000000 ) ;
#2611 = ORIENTED_EDGE ( 'NONE', *, *, #7401, .T. ) ;
#2612 = DIRECTION ( 'NONE',  ( -1.000000000000000000, 0.000000000000000000, 0.000000000000000000 ) ) ;
#2613 = DIRECTION ( 'NONE',  ( 1.000000000000000000, 0.000000000000000000, 0.000000000000000000 ) ) ;
#2614 = CIRCLE ( 'NONE', #2730, 4.171999999999995268 ) ;
#2615 = FACE_OUTER_BOUND ( 'NONE', #89, .T. ) ;
#2616 = DIRECTION ( 'NONE',  ( 1.000000000000000000, 0.000000000000000000, 0.000000000000000000 ) ) ;
#2617 = ORIENTED_EDGE ( 'NONE', *, *, #1372, .T. ) ;
#2618 = AXIS2_PLACEMENT_3D ( 'NONE', #5106, #5774, #6294 ) ;
#2619 = DIRECTION ( 'NONE',  ( 1.000000000000000000, -2.403401228516536951E-14, 0.000000000000000000 ) ) ;
#2620 = DIRECTION ( 'NONE',  ( -0.000000000000000000, -0.000000000000000000, 1.000000000000000000 ) ) ;
#2621 = DIRECTION ( 'NONE',  ( 0.000000000000000000, 0.000000000000000000, 1.000000000000000000 ) ) ;
#2622 = CIRCLE ( 'NONE', #1748, 30.30000000000000071 ) ;
#2623 = CARTESIAN_POINT ( 'NONE',  ( 4.000000000000005329, -6.928203230275506108, -4.700000000000000178 ) ) ;
#2624 = ORIENTED_EDGE ( 'NONE', *, *, #3553, .F. ) ;
#2625 = FACE_BOUND ( 'NONE', #5111, .T. ) ;
#2626 = CIRCLE ( 'NONE', #2749, 5.249999999999976907 ) ;
#2627 = FACE_OUTER_BOUND ( 'NONE', #5032, .T. ) ;
#2628 = EDGE_CURVE ( 'NONE', #5377, #719, #351, .T. ) ;
#2629 = DIRECTION ( 'NONE',  ( 0.000000000000000000, 0.000000000000000000, -1.000000000000000000 ) ) ;
#2630 = CARTESIAN_POINT ( 'NONE',  ( -5.000000000000000888, 6.123233995736767268E-16, 19.04999999999997229 ) ) ;
#2631 = CARTESIAN_POINT ( 'NONE',  ( -119.9981648402875578, 207.8429183184017859, 14.70000000000000462 ) ) ;
#2632 = AXIS2_PLACEMENT_3D ( 'NONE', #3773, #2629, #4395 ) ;
#2633 = CARTESIAN_POINT ( 'NONE',  ( 1.310872448937989931, -8.480771745766411129, -4.382649155111336903 ) ) ;
#2634 = LINE ( 'NONE', #7250, #4394 ) ;
#2635 = VERTEX_POINT ( 'NONE', #6278 ) ;
#2636 = ORIENTED_EDGE ( 'NONE', *, *, #138, .T. ) ;
#2637 = ADVANCED_FACE ( 'NONE', ( #2064 ), #2689, .F. ) ;
#2638 = EDGE_LOOP ( 'NONE', ( #659, #6792, #3594, #963 ) ) ;
#2639 = VECTOR ( 'NONE', #1764, 1000.000000000000000 ) ;
#2640 = DIRECTION ( 'NONE',  ( -1.000000000000000000, 0.000000000000000000, 0.000000000000000000 ) ) ;
#2641 = DIRECTION ( 'NONE',  ( -0.000000000000000000, -0.000000000000000000, -1.000000000000000000 ) ) ;
#2642 = CARTESIAN_POINT ( 'NONE',  ( 0.5700000000000001732, -28.49429942988597020, 0.000000000000000000 ) ) ;
#2643 =( NAMED_UNIT ( * ) SI_UNIT ( $, .STERADIAN. ) SOLID_ANGLE_UNIT ( ) );
#2644 = DIRECTION ( 'NONE',  ( -0.000000000000000000, -0.000000000000000000, 1.000000000000000000 ) ) ;
#2645 = EDGE_CURVE ( 'NONE', #1526, #6086, #1989, .T. ) ;
#2646 = VECTOR ( 'NONE', #4284, 1000.000000000000000 ) ;
#2647 = ORIENTED_EDGE ( 'NONE', *, *, #562, .F. ) ;
#2648 = EDGE_CURVE ( 'NONE', #2058, #3050, #829, .T. ) ;
#2649 = ORIENTED_EDGE ( 'NONE', *, *, #2992, .T. ) ;
#2650 = DIRECTION ( 'NONE',  ( -0.000000000000000000, -0.000000000000000000, 1.000000000000000000 ) ) ;
#2651 = EDGE_CURVE ( 'NONE', #520, #6904, #3242, .T. ) ;
#2652 = DIRECTION ( 'NONE',  ( 1.000000000000000000, 0.000000000000000000, 0.000000000000000000 ) ) ;
#2653 = ADVANCED_FACE ( 'NONE', ( #7490 ), #7455, .T. ) ;
#2654 = CYLINDRICAL_SURFACE ( 'NONE', #4058, 35.97500000000000853 ) ;
#2655 = ORIENTED_EDGE ( 'NONE', *, *, #2868, .F. ) ;
#2656 = AXIS2_PLACEMENT_3D ( 'NONE', #1863, #4813, #2427 ) ;
#2657 = EDGE_CURVE ( 'NONE', #2748, #7510, #1460, .T. ) ;
#2658 = DIRECTION ( 'NONE',  ( 0.9997999799959990108, -0.01999999999999999001, 0.000000000000000000 ) ) ;
#2659 = DIRECTION ( 'NONE',  ( 0.8660254037844382635, 0.5000000000000006661, 0.000000000000000000 ) ) ;
#2660 = AXIS2_PLACEMENT_3D ( 'NONE', #7683, #4133, #2298 ) ;
#2661 = DIRECTION ( 'NONE',  ( 3.081487911019577365E-33, -2.775557561562891967E-17, -1.000000000000000000 ) ) ;
#2662 = CARTESIAN_POINT ( 'NONE',  ( 0.000000000000000000, 0.000000000000000000, 0.000000000000000000 ) ) ;
#2663 = ORIENTED_EDGE ( 'NONE', *, *, #6365, .T. ) ;
#2664 = CIRCLE ( 'NONE', #4297, 29.99999999999999289 ) ;
#2665 = CARTESIAN_POINT ( 'NONE',  ( -213.0929183184026954, 119.9981648402859378, -50.00000000000000000 ) ) ;
#2666 = CARTESIAN_POINT ( 'NONE',  ( 0.000000000000000000, 0.000000000000000000, -3.000000000000000000 ) ) ;
#2667 = CARTESIAN_POINT ( 'NONE',  ( 89.90381056766652534, -74.99999999999882050, 0.000000000000000000 ) ) ;
#2668 = CARTESIAN_POINT ( 'NONE',  ( -29.99999999999999289, 3.673940397442058389E-15, -79.99999999999995737 ) ) ;
#2669 = APPLICATION_PROTOCOL_DEFINITION ( 'draft international standard', 'automotive_design', 1998, #6915 ) ;
#2670 = DIRECTION ( 'NONE',  ( 1.000000000000000000, 0.000000000000000000, 0.000000000000000000 ) ) ;
#2671 = ORIENTED_EDGE ( 'NONE', *, *, #4700, .F. ) ;
#2672 = ORIENTED_EDGE ( 'NONE', *, *, #362, .F. ) ;
#2673 = ORIENTED_EDGE ( 'NONE', *, *, #4171, .T. ) ;
#2674 = ORIENTED_EDGE ( 'NONE', *, *, #7409, .T. ) ;
#2675 = DIRECTION ( 'NONE',  ( 1.000000000000000000, 0.000000000000000000, 0.000000000000000000 ) ) ;
#2676 = DIRECTION ( 'NONE',  ( -0.000000000000000000, -0.000000000000000000, -1.000000000000000000 ) ) ;
#2677 = CARTESIAN_POINT ( 'NONE',  ( -114.7481648402868188, 207.8429183184021554, 10.00000000000000000 ) ) ;
#2678 = AXIS2_PLACEMENT_3D ( 'NONE', #7698, #5885, #5135 ) ;
#2679 = ORIENTED_EDGE ( 'NONE', *, *, #1727, .T. ) ;
#2680 = EDGE_CURVE ( 'NONE', #1325, #5846, #5680, .T. ) ;
#2681 = ORIENTED_EDGE ( 'NONE', *, *, #323, .T. ) ;
#2682 = ORIENTED_EDGE ( 'NONE', *, *, #6924, .T. ) ;
#2683 = ADVANCED_FACE ( 'NONE', ( #1606 ), #4011, .T. ) ;
#2684 = EDGE_CURVE ( 'NONE', #6492, #6903, #3013, .T. ) ;
#2685 = EDGE_CURVE ( 'NONE', #2582, #1983, #295, .T. ) ;
#2686 = CARTESIAN_POINT ( 'NONE',  ( -68.76644452187072432, 49.96174644486006855, -134.1720000000000255 ) ) ;
#2687 = EDGE_CURVE ( 'NONE', #4189, #6783, #4126, .T. ) ;
#2688 = DIRECTION ( 'NONE',  ( 1.000000000000000000, 0.000000000000000000, 0.000000000000000000 ) ) ;
#2689 = PLANE ( 'NONE',  #981 ) ;
#2690 =( REPRESENTATION_RELATIONSHIP ('NONE','NONE', #1229, #5768 ) REPRESENTATION_RELATIONSHIP_WITH_TRANSFORMATION ( #1078 )SHAPE_REPRESENTATION_RELATIONSHIP( ) );
#2691 = DIRECTION ( 'NONE',  ( 1.000000000000000000, 0.000000000000000000, 0.000000000000000000 ) ) ;
#2692 = AXIS2_PLACEMENT_3D ( 'NONE', #697, #4954, #1970 ) ;
#2693 = ORIENTED_EDGE ( 'NONE', *, *, #6062, .T. ) ;
#2694 = ADVANCED_FACE ( 'NONE', ( #1690 ), #7089, .T. ) ;
#2695 = CYLINDRICAL_SURFACE ( 'NONE', #7136, 279.9963296805736945 ) ;
#2696 = DIRECTION ( 'NONE',  ( 0.000000000000000000, 0.000000000000000000, -1.000000000000000000 ) ) ;
#2697 = VECTOR ( 'NONE', #7686, 1000.000000000000000 ) ;
#2698 = DIRECTION ( 'NONE',  ( 0.000000000000000000, 0.000000000000000000, 1.000000000000000000 ) ) ;
#2699 = DIRECTION ( 'NONE',  ( 0.000000000000000000, 0.000000000000000000, -1.000000000000000000 ) ) ;
#2700 = ORIENTED_EDGE ( 'NONE', *, *, #757, .F. ) ;
#2701 = AXIS2_PLACEMENT_3D ( 'NONE', #6370, #5261, #2740 ) ;
#2702 = DIRECTION ( 'NONE',  ( -0.000000000000000000, -0.000000000000000000, -1.000000000000000000 ) ) ;
#2703 = CARTESIAN_POINT ( 'NONE',  ( 10.00000000000000000, 28.28427124746189136, -139.9999999999999716 ) ) ;
#2704 = CARTESIAN_POINT ( 'NONE',  ( -68.76644452187068168, 49.96174644486002592, 0.000000000000000000 ) ) ;
#2705 = CARTESIAN_POINT ( 'NONE',  ( 8.000000000000000000, 4.618802153517004072, -4.700000000000000178 ) ) ;
#2706 = DIRECTION ( 'NONE',  ( -0.000000000000000000, -0.000000000000000000, 1.000000000000000000 ) ) ;
#2707 = SHAPE_DEFINITION_REPRESENTATION ( #7309, #2306 ) ;
#2708 = CIRCLE ( 'NONE', #3457, 2.250000000000001776 ) ;
#2709 = CIRCLE ( 'NONE', #1187, 5.249999999999976907 ) ;
#2710 = CARTESIAN_POINT ( 'NONE',  ( 0.000000000000000000, 0.000000000000000000, -93.00430309513780003 ) ) ;
#2711 = ORIENTED_EDGE ( 'NONE', *, *, #4964, .T. ) ;
#2712 = ORIENTED_EDGE ( 'NONE', *, *, #7228, .F. ) ;
#2713 = ORIENTED_EDGE ( 'NONE', *, *, #2886, .F. ) ;
#2714 = VERTEX_POINT ( 'NONE', #5991 ) ;
#2715 = ORIENTED_EDGE ( 'NONE', *, *, #2110, .F. ) ;
#2716 = DIRECTION ( 'NONE',  ( -0.000000000000000000, -0.000000000000000000, -1.000000000000000000 ) ) ;
#2717 = LINE ( 'NONE', #226, #5160 ) ;
#2718 = CARTESIAN_POINT ( 'NONE',  ( -5.134781488891348999E-13, 239.9963296805737230, -50.00000000000000000 ) ) ;
#2719 = ORIENTED_EDGE ( 'NONE', *, *, #1619, .F. ) ;
#2720 = ORIENTED_EDGE ( 'NONE', *, *, #5436, .F. ) ;
#2721 = AXIS2_PLACEMENT_3D ( 'NONE', #2738, #2042, #6216 ) ;
#2722 = ORIENTED_EDGE ( 'NONE', *, *, #5103, .T. ) ;
#2723 = CARTESIAN_POINT ( 'NONE',  ( -63.76644452187068879, 49.96174644486002592, -64.17200000000001125 ) ) ;
#2724 =( NAMED_UNIT ( * ) SI_UNIT ( $, .STERADIAN. ) SOLID_ANGLE_UNIT ( ) );
#2725 = DIRECTION ( 'NONE',  ( -0.000000000000000000, -0.000000000000000000, -1.000000000000000000 ) ) ;
#2726 = AXIS2_PLACEMENT_3D ( 'NONE', #5685, #6763, #166 ) ;
#2727 = CARTESIAN_POINT ( 'NONE',  ( -1.734723475976807094E-15, 9.237604307034017026, -0.7145311798163319628 ) ) ;
#2728 = EDGE_LOOP ( 'NONE', ( #2191, #4250 ) ) ;
#2729 = EDGE_CURVE ( 'NONE', #7759, #7346, #4272, .T. ) ;
#2730 = AXIS2_PLACEMENT_3D ( 'NONE', #1510, #801, #5025 ) ;
#2731 = CARTESIAN_POINT ( 'NONE',  ( 1.677050983124841466, 0.000000000000000000, 35.25000000000000000 ) ) ;
#2732 = CARTESIAN_POINT ( 'NONE',  ( 119.9981648402868899, 207.8429183184021269, -8.673617379884035472E-15 ) ) ;
#2733 = CARTESIAN_POINT ( 'NONE',  ( -3.200000000000008171, 3.673940397442059178E-15, 30.00000000000000000 ) ) ;
#2734 = CARTESIAN_POINT ( 'NONE',  ( -207.8429183184026670, 119.9981648402859378, -50.00000000000000000 ) ) ;
#2735 = EDGE_CURVE ( 'NONE', #3827, #3377, #4763, .T. ) ;
#2736 = ORIENTED_EDGE ( 'NONE', *, *, #5088, .T. ) ;
#2737 = CARTESIAN_POINT ( 'NONE',  ( -4.681546503268407275E-16, 9.237604307034017026, -4.700000000000000178 ) ) ;
#2738 = CARTESIAN_POINT ( 'NONE',  ( 0.000000000000000000, 0.000000000000000000, 0.000000000000000000 ) ) ;
#2739 = CIRCLE ( 'NONE', #7520, 28.50000000000000711 ) ;
#2740 = DIRECTION ( 'NONE',  ( -1.000000000000000000, 0.000000000000000000, 0.000000000000000000 ) ) ;
#2741 = B_SPLINE_CURVE_WITH_KNOTS ( 'NONE', 3,
 ( #236, #2028, #7345, #5014, #786, #7381, #6909, #4497 ),
 .UNSPECIFIED., .F., .F.,
 ( 4, 2, 2, 4 ),
 ( 0.004673709593152148775, 0.005837709341827643401, 0.007001709090503138028, 0.009329708587854127280 ),
 .UNSPECIFIED. ) ;
#2742 = CARTESIAN_POINT ( 'NONE',  ( 0.000000000000000000, 0.000000000000000000, -4.699999999999999289 ) ) ;
#2743 = CARTESIAN_POINT ( 'NONE',  ( 0.000000000000000000, 0.000000000000000000, -60.00000000000000711 ) ) ;
#2744 = ITEM_DEFINED_TRANSFORMATION ( 'NONE', 'NONE', #439,  #7485 ) ;
#2745 = EDGE_CURVE ( 'NONE', #1930, #5426, #7677, .T. ) ;
#2746 = CARTESIAN_POINT ( 'NONE',  ( 3.660532965668823469, -7.124194613927629760, -4.700000000000001066 ) ) ;
#2747 = ORIENTED_EDGE ( 'NONE', *, *, #6074, .F. ) ;
#2748 = VERTEX_POINT ( 'NONE', #28 ) ;
#2749 = AXIS2_PLACEMENT_3D ( 'NONE', #6123, #3130, #123 ) ;
#2750 = EDGE_CURVE ( 'NONE', #1651, #5807, #2957, .T. ) ;
#2751 = ORIENTED_EDGE ( 'NONE', *, *, #1427, .F. ) ;
#2752 = EDGE_CURVE ( 'NONE', #3955, #2329, #6898, .T. ) ;
#2753 = ORIENTED_EDGE ( 'NONE', *, *, #6264, .F. ) ;
#2754 = LINE ( 'NONE', #5189, #1681 ) ;
#2755 = CARTESIAN_POINT ( 'NONE',  ( -279.9963296805736945, 3.428966089163216048E-14, -50.00000000000004263 ) ) ;
#2756 = CARTESIAN_POINT ( 'NONE',  ( -73.76644452187066747, 49.96174644486002592, 0.000000000000000000 ) ) ;
#2757 = DIRECTION ( 'NONE',  ( 1.000000000000000000, 0.000000000000000000, 0.000000000000000000 ) ) ;
#2758 = CIRCLE ( 'NONE', #7162, 5.249999999999976907 ) ;
#2759 = CARTESIAN_POINT ( 'NONE',  ( -72.93844452187067873, 49.96174644486002592, -65.00000000000000000 ) ) ;
#2760 = ORIENTED_EDGE ( 'NONE', *, *, #5823, .T. ) ;
#2761 = CIRCLE ( 'NONE', #1494, 5.249999999999987566 ) ;
#2762 = ORIENTED_EDGE ( 'NONE', *, *, #5185, .F. ) ;
#2763 = ORIENTED_EDGE ( 'NONE', *, *, #3423, .T. ) ;
#2764 = DIRECTION ( 'NONE',  ( -0.000000000000000000, -0.000000000000000000, 1.000000000000000000 ) ) ;
#2765 = AXIS2_PLACEMENT_3D ( 'NONE', #1155, #646, #2512 ) ;
#2766 = CYLINDRICAL_SURFACE ( 'NONE', #2455, 30.00000000000000000 ) ;
#2767 = LINE ( 'NONE', #311, #2319 ) ;
#2768 = EDGE_LOOP ( 'NONE', ( #7339, #5182, #3112, #6048 ) ) ;
#2769 = EDGE_LOOP ( 'NONE', ( #30, #6012, #393, #5861 ) ) ;
#2770 = VECTOR ( 'NONE', #2374, 1000.000000000000000 ) ;
#2771 = CARTESIAN_POINT ( 'NONE',  ( 0.000000000000000000, 0.000000000000000000, 13.00000000000001066 ) ) ;
#2772 = CARTESIAN_POINT ( 'NONE',  ( 26.26644452187053957, 80.83980388508807380, 0.000000000000000000 ) ) ;
#2773 = CYLINDRICAL_SURFACE ( 'NONE', #4819, 28.49999999999999645 ) ;
#2774 = CIRCLE ( 'NONE', #5539, 5.249999999999976907 ) ;
#2775 = DIRECTION ( 'NONE',  ( 0.000000000000000000, 0.000000000000000000, -1.000000000000000000 ) ) ;
#2776 = ORIENTED_EDGE ( 'NONE', *, *, #4898, .T. ) ;
#2777 = ADVANCED_FACE ( 'NONE', ( #5359 ), #6502, .T. ) ;
#2778 = FACE_OUTER_BOUND ( 'NONE', #5832, .T. ) ;
#2779 = CIRCLE ( 'NONE', #4792, 5.250000000000004441 ) ;
#2780 = ADVANCED_FACE ( 'NONE', ( #2874 ), #1210, .T. ) ;
#2781 = EDGE_CURVE ( 'NONE', #1722, #2329, #3901, .T. ) ;
#2782 = LINE ( 'NONE', #3960, #3329 ) ;
#2783 = CARTESIAN_POINT ( 'NONE',  ( 10.00000000000000000, 33.54101966249685773, -50.00000000000000000 ) ) ;
#2784 = DIRECTION ( 'NONE',  ( 0.000000000000000000, 0.000000000000000000, 1.000000000000000000 ) ) ;
#2785 = CONTEXT_DEPENDENT_SHAPE_REPRESENTATION ( #1992, #251 ) ;
#2786 = ADVANCED_FACE ( 'NONE', ( #4047 ), #500, .F. ) ;
#2787 = CARTESIAN_POINT ( 'NONE',  ( -74.01644452187024115, -49.96174644486060856, 10.00000000000000000 ) ) ;
#2788 = CIRCLE ( 'NONE', #883, 28.50000000000000711 ) ;
#2789 = EDGE_LOOP ( 'NONE', ( #849, #2576 ) ) ;
#2790 = ORIENTED_EDGE ( 'NONE', *, *, #1380, .F. ) ;
#2791 = ORIENTED_EDGE ( 'NONE', *, *, #1375, .F. ) ;
#2792 = EDGE_CURVE ( 'NONE', #5001, #6427, #6671, .T. ) ;
#2793 = ORIENTED_EDGE ( 'NONE', *, *, #1486, .T. ) ;
#2794 = DIRECTION ( 'NONE',  ( -0.000000000000000000, -0.000000000000000000, 1.000000000000000000 ) ) ;
#2795 = APPLICATION_CONTEXT ( 'automotive_design' ) ;
#2796 = LINE ( 'NONE', #1005, #231 ) ;
#2797 = FACE_OUTER_BOUND ( 'NONE', #3560, .T. ) ;
#2798 = DIRECTION ( 'NONE',  ( 0.000000000000000000, 0.000000000000000000, 1.000000000000000000 ) ) ;
#2799 = DIRECTION ( 'NONE',  ( 1.000000000000000000, 0.000000000000000000, 0.000000000000000000 ) ) ;
#2800 = ORIENTED_EDGE ( 'NONE', *, *, #4755, .F. ) ;
#2801 = ORIENTED_EDGE ( 'NONE', *, *, #1522, .T. ) ;
#2802 = ORIENTED_EDGE ( 'NONE', *, *, #616, .F. ) ;
#2803 = LINE ( 'NONE', #5202, #6564 ) ;
#2804 = AXIS2_PLACEMENT_3D ( 'NONE', #7498, #912, #3179 ) ;
#2805 = PLANE ( 'NONE',  #7666 ) ;
#2806 = DIRECTION ( 'NONE',  ( 1.000000000000000000, 0.000000000000000000, 0.000000000000000000 ) ) ;
#2807 = EDGE_LOOP ( 'NONE', ( #4118, #858, #6624, #1797 ) ) ;
#2808 = VECTOR ( 'NONE', #4973, 1000.000000000000000 ) ;
#2809 = AXIS2_PLACEMENT_3D ( 'NONE', #213, #4950, #2045 ) ;
#2810 = DIRECTION ( 'NONE',  ( -0.000000000000000000, -0.000000000000000000, 1.000000000000000000 ) ) ;
#2811 = DIRECTION ( 'NONE',  ( 0.000000000000000000, 0.000000000000000000, -1.000000000000000000 ) ) ;
#2812 = CARTESIAN_POINT ( 'NONE',  ( -350.0000000000000000, -299.9999999999998863, -1041.954445729288636 ) ) ;
#2813 = VECTOR ( 'NONE', #604, 1000.000000000000000 ) ;
#2814 = FACE_OUTER_BOUND ( 'NONE', #4238, .T. ) ;
#2815 = ORIENTED_EDGE ( 'NONE', *, *, #7459, .T. ) ;
#2816 = CARTESIAN_POINT ( 'NONE',  ( 0.000000000000000000, 0.000000000000000000, -4.674599999999997202 ) ) ;
#2817 = AXIS2_PLACEMENT_3D ( 'NONE', #2965, #2884, #6591 ) ;
#2818 =( LENGTH_UNIT ( ) NAMED_UNIT ( * ) SI_UNIT ( .MILLI., .METRE. ) );
#2819 = DIRECTION ( 'NONE',  ( -0.000000000000000000, -0.000000000000000000, -1.000000000000000000 ) ) ;
#2820 = PLANE ( 'NONE',  #4265 ) ;
#2821 = CARTESIAN_POINT ( 'NONE',  ( 5.249999999999997335, 239.9963296805737230, 10.00000000000000000 ) ) ;
#2822 = CONTEXT_DEPENDENT_SHAPE_REPRESENTATION ( #6320, #4219 ) ;
#2823 = CARTESIAN_POINT ( 'NONE',  ( 0.000000000000000000, 1.484218055610305731, -3.000000000000000000 ) ) ;
#2824 = CIRCLE ( 'NONE', #5468, 30.00000000000000000 ) ;
#2825 = ORIENTED_EDGE ( 'NONE', *, *, #7176, .T. ) ;
#2826 = AXIS2_PLACEMENT_3D ( 'NONE', #1348, #6053, #5494 ) ;
#2827 = VERTEX_POINT ( 'NONE', #6579 ) ;
#2828 = ORIENTED_EDGE ( 'NONE', *, *, #878, .F. ) ;
#2829 = ADVANCED_FACE ( 'NONE', ( #3581 ), #4800, .T. ) ;
#2830 = LINE ( 'NONE', #4675, #6755 ) ;
#2831 = VECTOR ( 'NONE', #7286, 999.9999999999998863 ) ;
#2832 =( GEOMETRIC_REPRESENTATION_CONTEXT ( 3 ) GLOBAL_UNCERTAINTY_ASSIGNED_CONTEXT ( ( #1851 ) ) GLOBAL_UNIT_ASSIGNED_CONTEXT ( ( #347, #1414, #940 ) ) REPRESENTATION_CONTEXT ( 'NONE', 'WORKASPACE' ) );
#2833 = DIRECTION ( 'NONE',  ( 0.000000000000000000, 0.000000000000000000, -1.000000000000000000 ) ) ;
#2834 = DIRECTION ( 'NONE',  ( 0.000000000000000000, 0.000000000000000000, 1.000000000000000000 ) ) ;
#2835 = DIRECTION ( 'NONE',  ( 1.000000000000000000, 0.000000000000000000, 0.000000000000000000 ) ) ;
#2836 = FACE_OUTER_BOUND ( 'NONE', #1976, .T. ) ;
#2837 = DIRECTION ( 'NONE',  ( 1.000000000000000000, 0.000000000000000000, 0.000000000000000000 ) ) ;
#2838 = EDGE_CURVE ( 'NONE', #3509, #5165, #7209, .T. ) ;
#2839 = ORIENTED_EDGE ( 'NONE', *, *, #2061, .T. ) ;
#2840 = STYLED_ITEM ( 'NONE', ( #4407 ), #5288 ) ;
#2841 = ORIENTED_EDGE ( 'NONE', *, *, #2605, .T. ) ;
#2842 = ORIENTED_EDGE ( 'NONE', *, *, #3985, .F. ) ;
#2843 = CARTESIAN_POINT ( 'NONE',  ( -1.728922298134113098E-15, 8.513302795252935035E-16, 10.00000000000000000 ) ) ;
#2844 = AXIS2_PLACEMENT_3D ( 'NONE', #620, #5945, #5504 ) ;
#2845 = CARTESIAN_POINT ( 'NONE',  ( -78.76644452187068168, 49.96174644486002592, 0.000000000000000000 ) ) ;
#2846 = CARTESIAN_POINT ( 'NONE',  ( 0.000000000000000000, 0.000000000000000000, 2.573333333333333695 ) ) ;
#2847 = EDGE_LOOP ( 'NONE', ( #2720, #6760, #6965, #2679, #6443, #811 ) ) ;
#2848 = EDGE_CURVE ( 'NONE', #7033, #6826, #1812, .T. ) ;
#2849 = DIRECTION ( 'NONE',  ( 1.000000000000000000, 0.000000000000000000, 0.000000000000000000 ) ) ;
#2850 = DIRECTION ( 'NONE',  ( 0.000000000000000000, 0.000000000000000000, 1.000000000000000000 ) ) ;
#2851 = AXIS2_PLACEMENT_3D ( 'NONE', #6290, #955, #175 ) ;
#2852 = CARTESIAN_POINT ( 'NONE',  ( -207.8429183184020985, 119.9981648402869467, -8.673617379884035472E-15 ) ) ;
#2853 = CYLINDRICAL_SURFACE ( 'NONE', #1926, 5.249999999999997335 ) ;
#2854 = ORIENTED_EDGE ( 'NONE', *, *, #2781, .T. ) ;
#2855 = ORIENTED_EDGE ( 'NONE', *, *, #7451, .F. ) ;
#2856 = AXIS2_PLACEMENT_3D ( 'NONE', #5052, #201, #2619 ) ;
#2857 = CARTESIAN_POINT ( 'NONE',  ( -114.7481648402875578, 207.8429183184017859, -50.00000000000000000 ) ) ;
#2858 = CARTESIAN_POINT ( 'NONE',  ( 0.000000000000000000, 0.000000000000000000, 10.00000000000000000 ) ) ;
#2859 = FACE_BOUND ( 'NONE', #4066, .T. ) ;
#2860 = DIRECTION ( 'NONE',  ( 1.000000000000000000, 0.000000000000000000, 0.000000000000000000 ) ) ;
#2861 = DIRECTION ( 'NONE',  ( 0.000000000000000000, 0.000000000000000000, -1.000000000000000000 ) ) ;
#2862 = CONICAL_SURFACE ( 'NONE', #3869, 37.49999999999997868, 1.029744258676654090 ) ;
#2863 = FACE_OUTER_BOUND ( 'NONE', #5939, .T. ) ;
#2864 = ORIENTED_EDGE ( 'NONE', *, *, #6009, .T. ) ;
#2865 = VERTEX_POINT ( 'NONE', #5870 ) ;
#2866 = VERTEX_POINT ( 'NONE', #3736 ) ;
#2867 = AXIS2_PLACEMENT_3D ( 'NONE', #2912, #7129, #7049 ) ;
#2868 = EDGE_CURVE ( 'NONE', #1985, #2714, #656, .T. ) ;
#2869 = DIRECTION ( 'NONE',  ( -1.000000000000000000, 0.000000000000000000, 0.000000000000000000 ) ) ;
#2870 = CARTESIAN_POINT ( 'NONE',  ( 8.000000000000000000, 4.618802153517013842, -0.7145311798163319628 ) ) ;
#2871 = DIRECTION ( 'NONE',  ( 0.000000000000000000, 0.000000000000000000, 1.000000000000000000 ) ) ;
#2872 =( NAMED_UNIT ( * ) PLANE_ANGLE_UNIT ( ) SI_UNIT ( $, .RADIAN. ) );
#2873 = CARTESIAN_POINT ( 'NONE',  ( 28.32536770618215982, -3.150165759062971471, 10.00000000000000000 ) ) ;
#2874 = FACE_OUTER_BOUND ( 'NONE', #755, .T. ) ;
#2875 = CIRCLE ( 'NONE', #7149, 30.00000000000000000 ) ;
#2876 = ORIENTED_EDGE ( 'NONE', *, *, #2412, .F. ) ;
#2877 = ORIENTED_EDGE ( 'NONE', *, *, #3649, .T. ) ;
#2878 = ORIENTED_EDGE ( 'NONE', *, *, #6636, .T. ) ;
#2879 = AXIS2_PLACEMENT_3D ( 'NONE', #5020, #4428, #1424 ) ;
#2880 = DIRECTION ( 'NONE',  ( -5.551115123125782702E-17, 0.000000000000000000, -1.000000000000000000 ) ) ;
#2881 = CARTESIAN_POINT ( 'NONE',  ( -8.000000000000001776, -1.555946510856140996, -0.06708870216335509340 ) ) ;
#2882 = ADVANCED_FACE ( 'NONE', ( #6658, #4916, #6104 ), #6778, .T. ) ;
#2883 =( NAMED_UNIT ( * ) PLANE_ANGLE_UNIT ( ) SI_UNIT ( $, .RADIAN. ) );
#2884 = DIRECTION ( 'NONE',  ( -0.000000000000000000, -0.000000000000000000, -1.000000000000000000 ) ) ;
#2885 = VECTOR ( 'NONE', #1318, 1000.000000000000114 ) ;
#2886 = EDGE_CURVE ( 'NONE', #6434, #3299, #4322, .T. ) ;
#2887 = DIRECTION ( 'NONE',  ( -0.000000000000000000, -0.000000000000000000, 1.000000000000000000 ) ) ;
#2888 = VERTEX_POINT ( 'NONE', #1248 ) ;
#2889 = AXIS2_PLACEMENT_3D ( 'NONE', #4948, #4436, #6849 ) ;
#2890 = EDGE_CURVE ( 'NONE', #3506, #3664, #1285, .T. ) ;
#2891 = DIRECTION ( 'NONE',  ( -0.000000000000000000, -0.000000000000000000, -1.000000000000000000 ) ) ;
#2892 = CARTESIAN_POINT ( 'NONE',  ( -72.93844452187067873, 49.96174644486002592, 25.00000000000000000 ) ) ;
#2893 = CARTESIAN_POINT ( 'NONE',  ( -5.250000000000500933, 239.9963296805737230, -120.0000000000000000 ) ) ;
#2894 = CARTESIAN_POINT ( 'NONE',  ( 199.9963296805737230, -4.860399174643270382E-12, 10.00000000000000000 ) ) ;
#2895 = ADVANCED_FACE ( 'NONE', ( #6185, #4361 ), #4993, .T. ) ;
#2896 = ORIENTED_EDGE ( 'NONE', *, *, #3134, .F. ) ;
#2897 = CIRCLE ( 'NONE', #1376, 5.857142857142855874 ) ;
#2898 = ORIENTED_EDGE ( 'NONE', *, *, #843, .F. ) ;
#2899 = PLANE ( 'NONE',  #1340 ) ;
#2900 = SURFACE_STYLE_FILL_AREA ( #3994 ) ;
#2901 = CIRCLE ( 'NONE', #9, 7.999999999999998224 ) ;
#2902 = DIRECTION ( 'NONE',  ( 0.000000000000000000, 0.000000000000000000, -1.000000000000000000 ) ) ;
#2903 = PLANE ( 'NONE',  #6906 ) ;
#2904 = ITEM_DEFINED_TRANSFORMATION ( 'NONE', 'NONE', #2936,  #7485 ) ;
#2905 = CARTESIAN_POINT ( 'NONE',  ( 0.000000000000000000, 0.000000000000000000, 2.573333333332999739 ) ) ;
#2906 = EDGE_LOOP ( 'NONE', ( #1410, #6235, #1548, #5258 ) ) ;
#2907 = ORIENTED_EDGE ( 'NONE', *, *, #4259, .F. ) ;
#2908 = CIRCLE ( 'NONE', #2656, 37.49999999999997868 ) ;
#2909 = EDGE_LOOP ( 'NONE', ( #4888, #3977 ) ) ;
#2910 = CARTESIAN_POINT ( 'NONE',  ( -1.734723475976807094E-15, 9.237604307034017026, -3.985468820183668104 ) ) ;
#2911 = DIRECTION ( 'NONE',  ( 1.000000000000000000, 0.000000000000000000, 0.000000000000000000 ) ) ;
#2912 = CARTESIAN_POINT ( 'NONE',  ( -119.9981648402875578, 207.8429183184017859, -50.00000000000000000 ) ) ;
#2913 = DIRECTION ( 'NONE',  ( 0.000000000000000000, 0.000000000000000000, 1.000000000000000000 ) ) ;
#2914 = VECTOR ( 'NONE', #1135, 1000.000000000000000 ) ;
#2915 = DIRECTION ( 'NONE',  ( -0.000000000000000000, -0.000000000000000000, 1.000000000000000000 ) ) ;
#2916 = ORIENTED_EDGE ( 'NONE', *, *, #2927, .T. ) ;
#2917 = EDGE_LOOP ( 'NONE', ( #6895, #14 ) ) ;
#2918 = VECTOR ( 'NONE', #5002, 1000.000000000000000 ) ;
#2919 = VERTEX_POINT ( 'NONE', #6070 ) ;
#2920 = DIRECTION ( 'NONE',  ( 0.1305261922200541547, 0.9914448613738101601, -0.000000000000000000 ) ) ;
#2921 = FACE_BOUND ( 'NONE', #1159, .T. ) ;
#2922 = SHAPE_REPRESENTATION_RELATIONSHIP ( 'NONE' , 'NONE' ,  #2051, #5395 ) ;
#2923 = DIRECTION ( 'NONE',  ( -0.000000000000000000, -0.000000000000000000, 1.000000000000000000 ) ) ;
#2924 = EDGE_CURVE ( 'NONE', #4597, #926, #2897, .T. ) ;
#2925 = VERTEX_POINT ( 'NONE', #6144 ) ;
#2926 = EDGE_LOOP ( 'NONE', ( #3358, #5126, #2353, #6416 ) ) ;
#2927 = EDGE_CURVE ( 'NONE', #1526, #4732, #5655, .T. ) ;
#2928 = EDGE_CURVE ( 'NONE', #2748, #380, #7672, .T. ) ;
#2929 = EDGE_CURVE ( 'NONE', #719, #293, #7329, .T. ) ;
#2930 = CARTESIAN_POINT ( 'NONE',  ( -3.500000000000006661, 0.000000000000000000, 0.000000000000000000 ) ) ;
#2931 = DIRECTION ( 'NONE',  ( -1.000000000000000000, -0.000000000000000000, -0.000000000000000000 ) ) ;
#2932 = DIRECTION ( 'NONE',  ( 0.9845265360683707057, 0.1752355551171480841, 0.000000000000000000 ) ) ;
#2933 = FACE_OUTER_BOUND ( 'NONE', #3193, .T. ) ;
#2934 = AXIS2_PLACEMENT_3D ( 'NONE', #437, #5255, #2269 ) ;
#2935 = ORIENTED_EDGE ( 'NONE', *, *, #5238, .T. ) ;
#2936 = AXIS2_PLACEMENT_3D ( 'NONE', #7285, #1887, #6693 ) ;
#2937 = ORIENTED_EDGE ( 'NONE', *, *, #4071, .F. ) ;
#2938 = EDGE_CURVE ( 'NONE', #147, #688, #4907, .T. ) ;
#2939 = CARTESIAN_POINT ( 'NONE',  ( 5.249999999999992895, 239.9963296805737230, -8.673617379884035472E-15 ) ) ;
#2940 = CARTESIAN_POINT ( 'NONE',  ( -63.76644452187068879, 49.96174644486002592, 24.17200000000001125 ) ) ;
#2941 = DIRECTION ( 'NONE',  ( 0.000000000000000000, 0.000000000000000000, 1.000000000000000000 ) ) ;
#2942 = AXIS2_PLACEMENT_3D ( 'NONE', #3014, #7231, #598 ) ;
#2943 = DIRECTION ( 'NONE',  ( 0.000000000000000000, 0.000000000000000000, 1.000000000000000000 ) ) ;
#2944 = FACE_BOUND ( 'NONE', #1861, .T. ) ;
#2945 = DIRECTION ( 'NONE',  ( 0.000000000000000000, 0.000000000000000000, -1.000000000000000000 ) ) ;
#2946 = DIRECTION ( 'NONE',  ( 1.000000000000000000, 0.000000000000000000, 0.000000000000000000 ) ) ;
#2947 = ORIENTED_EDGE ( 'NONE', *, *, #1929, .T. ) ;
#2948 = APPLICATION_CONTEXT ( 'automotive_design' ) ;
#2949 = ORIENTED_EDGE ( 'NONE', *, *, #6385, .T. ) ;
#2950 = VECTOR ( 'NONE', #4917, 1000.000000000000000 ) ;
#2951 = CARTESIAN_POINT ( 'NONE',  ( -6.686525924292790357, 5.377136764700156668, -4.383279549040164369 ) ) ;
#2952 = CARTESIAN_POINT ( 'NONE',  ( -5.459126460941067016, -34.89491303563345070, -3.000000000000000000 ) ) ;
#2953 = DIRECTION ( 'NONE',  ( 1.000000000000000000, 0.000000000000000000, 0.000000000000000000 ) ) ;
#2954 = CARTESIAN_POINT ( 'NONE',  ( 26.26644452186938850, 80.83980388508842907, -54.70000000000000284 ) ) ;
#2955 = VECTOR ( 'NONE', #2923, 1000.000000000000000 ) ;
#2956 = DIRECTION ( 'NONE',  ( 0.000000000000000000, 0.000000000000000000, -1.000000000000000000 ) ) ;
#2957 = LINE ( 'NONE', #4089, #1628 ) ;
#2958 = ORIENTED_EDGE ( 'NONE', *, *, #4275, .T. ) ;
#2959 = EDGE_LOOP ( 'NONE', ( #1002, #4901, #156, #5767 ) ) ;
#2960 = AXIS2_PLACEMENT_3D ( 'NONE', #791, #3210, #5532 ) ;
#2961 = EDGE_LOOP ( 'NONE', ( #6146, #3172 ) ) ;
#2962 = CARTESIAN_POINT ( 'NONE',  ( -199.9963296805737230, 0.000000000000000000, 10.00000000000000000 ) ) ;
#2963 = CARTESIAN_POINT ( 'NONE',  ( -10.00000000000000000, 0.000000000000000000, 0.000000000000000000 ) ) ;
#2964 =( LENGTH_UNIT ( ) NAMED_UNIT ( * ) SI_UNIT ( .MILLI., .METRE. ) );
#2965 = CARTESIAN_POINT ( 'NONE',  ( 0.000000000000000000, 0.000000000000000000, 10.00000000000000000 ) ) ;
#2966 = AXIS2_PLACEMENT_3D ( 'NONE', #214, #921, #7550 ) ;
#2967 = ORIENTED_EDGE ( 'NONE', *, *, #6359, .T. ) ;
#2968 = ORIENTED_EDGE ( 'NONE', *, *, #6542, .F. ) ;
#2969 = AXIS2_PLACEMENT_3D ( 'NONE', #2212, #5193, #2757 ) ;
#2970 = DIRECTION ( 'NONE',  ( -1.000000000000000000, 0.000000000000000000, 0.000000000000000000 ) ) ;
#2971 = DIRECTION ( 'NONE',  ( -5.551115123125782702E-17, 0.000000000000000000, -1.000000000000000000 ) ) ;
#2972 = DIRECTION ( 'NONE',  ( 0.000000000000000000, 0.000000000000000000, 1.000000000000000000 ) ) ;
#2973 = CARTESIAN_POINT ( 'NONE',  ( 207.8429183184021269, 119.9981648402868331, -50.00000000000000000 ) ) ;
#2974 = ORIENTED_EDGE ( 'NONE', *, *, #5133, .T. ) ;
#2975 = EDGE_CURVE ( 'NONE', #1710, #6167, #103, .T. ) ;
#2976 = EDGE_LOOP ( 'NONE', ( #4159, #533, #4065, #5337 ) ) ;
#2977 = ORIENTED_EDGE ( 'NONE', *, *, #4424, .F. ) ;
#2978=STYLED_ITEM('',(#7809),#525);
#2979 = PLANE ( 'NONE',  #5248 ) ;
#2980 = DIRECTION ( 'NONE',  ( -0.000000000000000000, -0.000000000000000000, 1.000000000000000000 ) ) ;
#2981 = FACE_BOUND ( 'NONE', #848, .T. ) ;
#2982 = CARTESIAN_POINT ( 'NONE',  ( -37.49999999999997868, 4.592425496802572000E-15, -90.00000000000000000 ) ) ;
#2983 = ITEM_DEFINED_TRANSFORMATION ( 'NONE', 'NONE', #5862,  #7485 ) ;
#2984 = ADVANCED_FACE ( 'NONE', ( #1923 ), #238, .T. ) ;
#2985 = DIRECTION ( 'NONE',  ( 1.000000000000000000, 0.000000000000000000, 0.000000000000000000 ) ) ;
#2986 = PRODUCT_DEFINITION_CONTEXT ( 'detailed design', #2040, 'design' ) ;
#2987 = ORIENTED_EDGE ( 'NONE', *, *, #5198, .F. ) ;
#2988 = VECTOR ( 'NONE', #3643, 1000.000000000000000 ) ;
#2989 = ADVANCED_FACE ( 'NONE', ( #3228 ), #7397, .T. ) ;
#2990 = ORIENTED_EDGE ( 'NONE', *, *, #5576, .T. ) ;
#2991 = CARTESIAN_POINT ( 'NONE',  ( 5.355005115540896199, 6.145890662064656063, -4.617753204360287356 ) ) ;
#2992 = EDGE_CURVE ( 'NONE', #3509, #924, #6419, .T. ) ;
#2993 = VECTOR ( 'NONE', #6884, 1000.000000000000000 ) ;
#2994 = DIRECTION ( 'NONE',  ( -0.9987587364483917485, -0.04980950078059114688, 0.000000000000000000 ) ) ;
#2995 = DIRECTION ( 'NONE',  ( 0.000000000000000000, 0.000000000000000000, -1.000000000000000000 ) ) ;
#2996 = CARTESIAN_POINT ( 'NONE',  ( 85.00000000000000000, 9.922618282587336580E-13, -54.70000000000000284 ) ) ;
#2997 = CARTESIAN_POINT ( 'NONE',  ( 0.000000000000000000, 0.000000000000000000, 0.000000000000000000 ) ) ;
#2998 = EDGE_CURVE ( 'NONE', #6427, #5001, #5917, .T. ) ;
#2999 = ORIENTED_EDGE ( 'NONE', *, *, #2924, .F. ) ;
#3000 = VECTOR ( 'NONE', #4515, 1000.000000000000000 ) ;
#3001 = VERTEX_POINT ( 'NONE', #1969 ) ;
#3002 = ORIENTED_EDGE ( 'NONE', *, *, #3174, .F. ) ;
#3003 = DIRECTION ( 'NONE',  ( 0.000000000000000000, 0.000000000000000000, -1.000000000000000000 ) ) ;
#3004 = CARTESIAN_POINT ( 'NONE',  ( -68.76644452187068168, 49.96174644486002592, -40.00000000000000000 ) ) ;
#3005 = AXIS2_PLACEMENT_3D ( 'NONE', #320, #909, #836 ) ;
#3006 = CARTESIAN_POINT ( 'NONE',  ( -279.9963296805736945, 3.428966089163216048E-14, -50.00000000000004263 ) ) ;
#3007 = ORIENTED_EDGE ( 'NONE', *, *, #2568, .T. ) ;
#3008 = VERTEX_POINT ( 'NONE', #216 ) ;
#3009 = VECTOR ( 'NONE', #5214, 1000.000000000000000 ) ;
#3010 = DIRECTION ( 'NONE',  ( -1.000000000000000000, 0.000000000000000000, 0.000000000000000000 ) ) ;
#3011 = VECTOR ( 'NONE', #6575, 1000.000000000000000 ) ;
#3012 = CARTESIAN_POINT ( 'NONE',  ( 125.2481648402868615, 207.8429183184021269, 10.00000000000000178 ) ) ;
#3013 = CIRCLE ( 'NONE', #7414, 4.250000000000000000 ) ;
#3014 = CARTESIAN_POINT ( 'NONE',  ( -119.9981648402868046, 207.8429183184021554, 10.00000000000000178 ) ) ;
#3015 = ORIENTED_EDGE ( 'NONE', *, *, #2116, .T. ) ;
#3016 = VECTOR ( 'NONE', #5734, 1000.000000000000000 ) ;
#3017 = ORIENTED_EDGE ( 'NONE', *, *, #4529, .T. ) ;
#3018 = CARTESIAN_POINT ( 'NONE',  ( 3.500000000000006661, 0.000000000000000000, 0.000000000000000000 ) ) ;
#3019 = LINE ( 'NONE', #18, #5201 ) ;
#3020 = PLANE ( 'NONE',  #617 ) ;
#3021 = CARTESIAN_POINT ( 'NONE',  ( 3.716043017018883621, 28.25669875083898930, 13.00000000000000178 ) ) ;
#3022 = AXIS2_PLACEMENT_3D ( 'NONE', #3004, #7723, #4095 ) ;
#3023 = CARTESIAN_POINT ( 'NONE',  ( -202.5929183184021269, 119.9981648402869467, 10.00000000000000000 ) ) ;
#3024 = ORIENTED_EDGE ( 'NONE', *, *, #3124, .F. ) ;
#3025 = EDGE_CURVE ( 'NONE', #1610, #3551, #2634, .T. ) ;
#3026 = EDGE_CURVE ( 'NONE', #4169, #669, #2404, .T. ) ;
#3027=STYLED_ITEM('',(#7809),#3160);
#3028 = EDGE_CURVE ( 'NONE', #5001, #1502, #3262, .T. ) ;
#3029 = LINE ( 'NONE', #2558, #6307 ) ;
#3030 = EDGE_CURVE ( 'NONE', #7307, #6615, #7423, .T. ) ;
#3031 = CYLINDRICAL_SURFACE ( 'NONE', #1759, 5.249999999999991118 ) ;
#3032 = LINE ( 'NONE', #2003, #5257 ) ;
#3033 = DIRECTION ( 'NONE',  ( 0.000000000000000000, 0.000000000000000000, 1.000000000000000000 ) ) ;
#3034 = PRODUCT_DEFINITION_SHAPE ( 'NONE', 'NONE',  #7778 ) ;
#3035 =( NAMED_UNIT ( * ) PLANE_ANGLE_UNIT ( ) SI_UNIT ( $, .RADIAN. ) );
#3036 = CARTESIAN_POINT ( 'NONE',  ( -73.76644452187072432, 49.96174644486006855, -40.00000000000000000 ) ) ;
#3038 = CIRCLE ( 'NONE', #7430, 5.250000000000000888 ) ;
#3037 = FACE_BOUND ( 'NONE', #2257, .T. ) ;
#3039 = EDGE_LOOP ( 'NONE', ( #118, #3859, #281, #1362 ) ) ;
#3040 = ADVANCED_FACE ( 'NONE', ( #253 ), #5031, .F. ) ;
#3041 = ORIENTED_EDGE ( 'NONE', *, *, #2568, .F. ) ;
#3042 = ORIENTED_EDGE ( 'NONE', *, *, #5245, .T. ) ;
#3043 = AXIS2_PLACEMENT_3D ( 'NONE', #2308, #7729, #478 ) ;
#3044 = CARTESIAN_POINT ( 'NONE',  ( 5.000000000000000888, 0.000000000000000000, 19.04999999999997229 ) ) ;
#3045 = FACE_OUTER_BOUND ( 'NONE', #7561, .T. ) ;
#3046 = SURFACE_STYLE_USAGE ( .BOTH. , #4176 ) ;
#3047 = DIRECTION ( 'NONE',  ( -0.000000000000000000, -0.000000000000000000, -1.000000000000000000 ) ) ;
#3048 = EDGE_LOOP ( 'NONE', ( #7092, #492, #4325, #745 ) ) ;
#3049 = CIRCLE ( 'NONE', #7442, 5.250000000000004441 ) ;
#3050 = VERTEX_POINT ( 'NONE', #4729 ) ;
#3051 = CARTESIAN_POINT ( 'NONE',  ( 3.199999999999996181, 0.000000000000000000, 0.000000000000000000 ) ) ;
#3052 = CARTESIAN_POINT ( 'NONE',  ( -2.081668171172168513E-14, -9.237604307034017026, -0.7145311798163319628 ) ) ;
#3053 = DIRECTION ( 'NONE',  ( 3.081487911019577365E-33, -2.775557561562891967E-17, -1.000000000000000000 ) ) ;
#3054 = VERTEX_POINT ( 'NONE', #1818 ) ;
#3055 = ORIENTED_EDGE ( 'NONE', *, *, #3850, .T. ) ;
#3056 = CARTESIAN_POINT ( 'NONE',  ( -28.05900627794857272, -4.994213320838722936, -82.99999999999995737 ) ) ;
#3057 = LINE ( 'NONE', #4348, #5595 ) ;
#3058 = DIRECTION ( 'NONE',  ( 1.000000000000000000, 0.000000000000000000, 0.000000000000000000 ) ) ;
#3059 = FACE_OUTER_BOUND ( 'NONE', #5067, .T. ) ;
#3060 = AXIS2_PLACEMENT_3D ( 'NONE', #2555, #4943, #2699 ) ;
#3061 = FACE_BOUND ( 'NONE', #4149, .T. ) ;
#3062 = ORIENTED_EDGE ( 'NONE', *, *, #2592, .F. ) ;
#3063 = AXIS2_PLACEMENT_3D ( 'NONE', #5416, #3676, #46 ) ;
#3064 = PRODUCT_DEFINITION_FORMATION_WITH_SPECIFIED_SOURCE ( 'ANY', '', #3721, .NOT_KNOWN. ) ;
#3065 = CARTESIAN_POINT ( 'NONE',  ( -73.76644452187066747, 49.96174644486002592, -64.17200000000001125 ) ) ;
#3066 = FACE_BOUND ( 'NONE', #2909, .T. ) ;
#3067 = PLANE ( 'NONE',  #6521 ) ;
#3068 = DIRECTION ( 'NONE',  ( 0.000000000000000000, 0.000000000000000000, -1.000000000000000000 ) ) ;
#3069 = CARTESIAN_POINT ( 'NONE',  ( -1.677050983124841466, 0.000000000000000000, 0.000000000000000000 ) ) ;
#3070 = VECTOR ( 'NONE', #2450, 1000.000000000000000 ) ;
#3071 = DIRECTION ( 'NONE',  ( 0.000000000000000000, 0.000000000000000000, -1.000000000000000000 ) ) ;
#3072 = ORIENTED_EDGE ( 'NONE', *, *, #6264, .T. ) ;
#3073 = EDGE_CURVE ( 'NONE', #5822, #7440, #5790, .T. ) ;
#3074 = ORIENTED_EDGE ( 'NONE', *, *, #7182, .F. ) ;
#3075 = EDGE_LOOP ( 'NONE', ( #6128, #4726 ) ) ;
#3076 = CIRCLE ( 'NONE', #4329, 6.099504629071905271 ) ;
#3077 = DIRECTION ( 'NONE',  ( 1.000000000000000000, 0.000000000000000000, 0.000000000000000000 ) ) ;
#3078 = CARTESIAN_POINT ( 'NONE',  ( 7.345652830558762503, -4.996589667937383794, -4.203584543331203349 ) ) ;
#3079 = SURFACE_SIDE_STYLE ('',( #76 ) ) ;
#3080 = DIRECTION ( 'NONE',  ( 0.8191520442889924647, 1.003171929053525486E-16, -0.5735764363510451602 ) ) ;
#3081 = ADVANCED_FACE ( 'NONE', ( #1746, #3045 ), #7179, .F. ) ;
#3082 = AXIS2_PLACEMENT_3D ( 'NONE', #2055, #2608, #969 ) ;
#3083 = ORIENTED_EDGE ( 'NONE', *, *, #4067, .F. ) ;
#3084 = AXIS2_PLACEMENT_3D ( 'NONE', #2772, #1544, #1467 ) ;
#3085 = ORIENTED_EDGE ( 'NONE', *, *, #1583, .T. ) ;
#3086 = FACE_OUTER_BOUND ( 'NONE', #1509, .T. ) ;
#3088 = PRESENTATION_LAYER_ASSIGNMENT (  '', '', ( #429 ) ) ;
#3087 = CARTESIAN_POINT ( 'NONE',  ( -28.49999999999999645, 3.490243377569956456E-15, -3.000000000000000000 ) ) ;
#3089 = AXIS2_PLACEMENT_3D ( 'NONE', #1033, #2541, #7117 ) ;
#3090 = DIRECTION ( 'NONE',  ( 0.01999999999999999001, 0.9997999799959990108, -0.000000000000000000 ) ) ;
#3091 = DIRECTION ( 'NONE',  ( -1.000000000000000000, 0.000000000000000000, 0.000000000000000000 ) ) ;
#3092 = ORIENTED_EDGE ( 'NONE', *, *, #5346, .F. ) ;
#3093 = EDGE_CURVE ( 'NONE', #3738, #4221, #119, .T. ) ;
#3094 = ORIENTED_EDGE ( 'NONE', *, *, #5388, .F. ) ;
#3095 = PRODUCT_DEFINITION_SHAPE ( 'NONE', 'NONE',  #7789 ) ;
#3096 =( REPRESENTATION_RELATIONSHIP ('NONE','NONE', #1229, #7725 ) REPRESENTATION_RELATIONSHIP_WITH_TRANSFORMATION ( #2904 )SHAPE_REPRESENTATION_RELATIONSHIP( ) );
#3097 = CARTESIAN_POINT ( 'NONE',  ( -279.9963296805736945, 3.428966089163216048E-14, -82.99999999999998579 ) ) ;
#3098 = CYLINDRICAL_SURFACE ( 'NONE', #3437, 29.99999999999999289 ) ;
#3099 = LINE ( 'NONE', #5495, #234 ) ;
#3100 = DIRECTION ( 'NONE',  ( -0.000000000000000000, -0.000000000000000000, 1.000000000000000000 ) ) ;
#3101 = CARTESIAN_POINT ( 'NONE',  ( 0.000000000000000000, 0.000000000000000000, -90.00000000000000000 ) ) ;
#3102 = CIRCLE ( 'NONE', #823, 28.50000000000000711 ) ;
#3103 = ORIENTED_EDGE ( 'NONE', *, *, #6610, .F. ) ;
#3104 = CARTESIAN_POINT ( 'NONE',  ( 0.000000000000000000, 0.000000000000000000, 0.000000000000000000 ) ) ;
#3105 = FACE_BOUND ( 'NONE', #7700, .T. ) ;
#3106 = CARTESIAN_POINT ( 'NONE',  ( -0.3344772040064616925, 4.405666859932604686E-15, -35.97500000000000853 ) ) ;
#3107 = CARTESIAN_POINT ( 'NONE',  ( -119.9981648402862646, 122.8429183184016864, 0.000000000000000000 ) ) ;
#3108 = VECTOR ( 'NONE', #603, 1000.000000000000000 ) ;
#3109 = CARTESIAN_POINT ( 'NONE',  ( -5.459126460941067016, -34.89491303563345070, 0.000000000000000000 ) ) ;
#3110 = DIRECTION ( 'NONE',  ( -1.000000000000000000, 0.000000000000000000, -0.000000000000000000 ) ) ;
#3111 = DIRECTION ( 'NONE',  ( 1.000000000000000000, 0.000000000000000000, 0.000000000000000000 ) ) ;
#3112 = ORIENTED_EDGE ( 'NONE', *, *, #1525, .T. ) ;
#3113 = ORIENTED_EDGE ( 'NONE', *, *, #3122, .F. ) ;
#3114 = ADVANCED_FACE ( 'NONE', ( #2921, #3588 ), #467, .F. ) ;
#3115 = CIRCLE ( 'NONE', #1218, 2.250000000000001776 ) ;
#3116 = EDGE_LOOP ( 'NONE', ( #3340, #4935, #7333, #635, #613, #2987, #4400, #4921 ) ) ;
#3117 = DIRECTION ( 'NONE',  ( 1.000000000000000000, 0.000000000000000000, 0.000000000000000000 ) ) ;
#3118 = DIRECTION ( 'NONE',  ( -0.000000000000000000, -0.000000000000000000, 1.000000000000000000 ) ) ;
#3119 = CYLINDRICAL_SURFACE ( 'NONE', #3705, 28.50000000000000711 ) ;
#3120 = AXIS2_PLACEMENT_3D ( 'NONE', #6027, #26, #2126 ) ;
#3121 = VERTEX_POINT ( 'NONE', #5997 ) ;
#3122 = EDGE_CURVE ( 'NONE', #3787, #7537, #6174, .T. ) ;
#3123 = VERTEX_POINT ( 'NONE', #7057 ) ;
#3124 = EDGE_CURVE ( 'NONE', #5462, #7689, #4556, .T. ) ;
#3125 = ADVANCED_FACE ( 'NONE', ( #7684 ), #4530, .T. ) ;
#3126 = AXIS2_PLACEMENT_3D ( 'NONE', #6016, #7315, #4308 ) ;
#3127 = CARTESIAN_POINT ( 'NONE',  ( -5.846731056662405557, 29.42474699893032053, -82.99999999999995737 ) ) ;
#3128 = CARTESIAN_POINT ( 'NONE',  ( -8.000000000000000000, -4.618802153517013842, -3.985468820183668104 ) ) ;
#3129 = EDGE_CURVE ( 'NONE', #7232, #4531, #5407, .T. ) ;
#3130 = DIRECTION ( 'NONE',  ( -0.000000000000000000, -0.000000000000000000, 1.000000000000000000 ) ) ;
#3131 = CARTESIAN_POINT ( 'NONE',  ( 8.000000000000000000, -0.7805016046290993437, -4.700000000000000178 ) ) ;
#3132 = VERTEX_POINT ( 'NONE', #6629 ) ;
#3133 = AXIS2_PLACEMENT_3D ( 'NONE', #402, #7119, #1717 ) ;
#3134 = EDGE_CURVE ( 'NONE', #5121, #7260, #3648, .T. ) ;
#3135 = ORIENTED_EDGE ( 'NONE', *, *, #3030, .F. ) ;
#3136 = DIRECTION ( 'NONE',  ( -0.000000000000000000, -0.000000000000000000, 1.000000000000000000 ) ) ;
#3137 = CARTESIAN_POINT ( 'NONE',  ( -4.665299213380359689, 29.63502966507089909, -82.99999999999995737 ) ) ;
#3138 = CIRCLE ( 'NONE', #6788, 8.000000000000000000 ) ;
#3139 = CARTESIAN_POINT ( 'NONE',  ( 31.51644452187053602, 80.83980388508807380, 0.000000000000000000 ) ) ;
#3140 = FACE_BOUND ( 'NONE', #2244, .T. ) ;
#3141 = ADVANCED_FACE ( 'NONE', ( #506 ), #1698, .T. ) ;
#3142 = DIRECTION ( 'NONE',  ( 0.000000000000000000, 0.000000000000000000, 1.000000000000000000 ) ) ;
#3143 = EDGE_LOOP ( 'NONE', ( #4610, #6396, #3626, #440 ) ) ;
#3144 = VECTOR ( 'NONE', #4044, 1000.000000000000000 ) ;
#3145 = MANIFOLD_SOLID_BREP ( 'TorqueElement', #1452 ) ;
#3146 = AXIS2_PLACEMENT_3D ( 'NONE', #1595, #3488, #7038 ) ;
#3147 = CARTESIAN_POINT ( 'NONE',  ( -119.9981648402875578, 207.8429183184017859, -50.00000000000000000 ) ) ;
#3148 = DIRECTION ( 'NONE',  ( 1.000000000000000000, 0.000000000000000000, 0.000000000000000000 ) ) ;
#3149 = SHAPE_DEFINITION_REPRESENTATION ( #1195, #420 ) ;
#3150 = FILL_AREA_STYLE_COLOUR ( '', #6729 ) ;
#3151 = CARTESIAN_POINT ( 'NONE',  ( 0.000000000000000000, 0.000000000000000000, 10.00000000000000000 ) ) ;
#3152 = DIRECTION ( 'NONE',  ( 1.000000000000000000, 0.000000000000000000, 0.000000000000000000 ) ) ;
#3153 = VERTEX_POINT ( 'NONE', #151 ) ;
#3154 = AXIS2_PLACEMENT_3D ( 'NONE', #2380, #4052, #5915 ) ;
#3155 = ORIENTED_EDGE ( 'NONE', *, *, #2116, .F. ) ;
#3156 = ORIENTED_EDGE ( 'NONE', *, *, #2312, .F. ) ;
#3157 = CYLINDRICAL_SURFACE ( 'NONE', #16, 5.000000000000000888 ) ;
#3158 = PRESENTATION_STYLE_ASSIGNMENT (( #2572 ) ) ;
#3159 = CONICAL_SURFACE ( 'NONE', #6930, 8.000000000000000000, 1.047197551196596299 ) ;
#3160 = MANIFOLD_SOLID_BREP ( 'M10 Clearance Hole1', #2098 ) ;
#3161 = DIRECTION ( 'NONE',  ( -0.000000000000000000, 1.000000000000000000, 0.000000000000000000 ) ) ;
#3162 = ORIENTED_EDGE ( 'NONE', *, *, #3406, .T. ) ;
#3163 = PRODUCT_DEFINITION_SHAPE ( 'NONE', 'NONE',  #7779 ) ;
#3164 = ORIENTED_EDGE ( 'NONE', *, *, #4992, .T. ) ;
#3165 = ORIENTED_EDGE ( 'NONE', *, *, #7647, .T. ) ;
#3166 = FACE_OUTER_BOUND ( 'NONE', #8, .T. ) ;
#3167 = SURFACE_SIDE_STYLE ('',( #161 ) ) ;
#3168 = EDGE_CURVE ( 'NONE', #6375, #6313, #6911, .T. ) ;
#3169 = CARTESIAN_POINT ( 'NONE',  ( -0.5700000000000001732, -28.49429942988597020, -3.000000000000000000 ) ) ;
#3170 = CIRCLE ( 'NONE', #7195, 30.30000000000000071 ) ;
#3171 = CARTESIAN_POINT ( 'NONE',  ( -1.728922298134113098E-15, 8.513302795252935035E-16, 13.00000000000000178 ) ) ;
#3172 = ORIENTED_EDGE ( 'NONE', *, *, #4371, .T. ) ;
#3173 = EDGE_CURVE ( 'NONE', #5558, #5183, #740, .T. ) ;
#3174 = EDGE_CURVE ( 'NONE', #544, #6148, #1001, .T. ) ;
#3175 = ORIENTED_EDGE ( 'NONE', *, *, #1629, .F. ) ;
#3176 = DIRECTION ( 'NONE',  ( 1.000000000000000000, 0.000000000000000000, 0.000000000000000000 ) ) ;
#3177 = CARTESIAN_POINT ( 'NONE',  ( 0.000000000000000000, 0.000000000000000000, -4.674599999999997202 ) ) ;
#3178 = FACE_BOUND ( 'NONE', #5070, .T. ) ;
#3179 = DIRECTION ( 'NONE',  ( 1.000000000000000000, 0.000000000000000000, 0.000000000000000000 ) ) ;
#3180 = EDGE_CURVE ( 'NONE', #6741, #5661, #5794, .T. ) ;
#3181 = VERTEX_POINT ( 'NONE', #2457 ) ;
#3182 = CARTESIAN_POINT ( 'NONE',  ( 5.249999999999477751, 239.9963296805737230, -50.00000000000000000 ) ) ;
#3183 = MANIFOLD_SOLID_BREP ( 'Mirror1', #5858 ) ;
#3184 = DIRECTION ( 'NONE',  ( 0.000000000000000000, 0.000000000000000000, 1.000000000000000000 ) ) ;
#3185 = VECTOR ( 'NONE', #3805, 1000.000000000000000 ) ;
#3186 = DIRECTION ( 'NONE',  ( -0.000000000000000000, -0.000000000000000000, 1.000000000000000000 ) ) ;
#3187 = PLANE ( 'NONE',  #5387 ) ;
#3188 = DIRECTION ( 'NONE',  ( 0.000000000000000000, 0.000000000000000000, 1.000000000000000000 ) ) ;
#3189 = VECTOR ( 'NONE', #5540, 1000.000000000000000 ) ;
#3190 = ORIENTED_EDGE ( 'NONE', *, *, #6553, .F. ) ;
#3191 = AXIS2_PLACEMENT_3D ( 'NONE', #1320, #4990, #6813 ) ;
#3192 = VERTEX_POINT ( 'NONE', #7257 ) ;
#3193 = EDGE_LOOP ( 'NONE', ( #6194, #2431 ) ) ;
#3194 = CARTESIAN_POINT ( 'NONE',  ( 0.000000000000000000, 0.000000000000000000, -3.000000000000000000 ) ) ;
#3195 = FILL_AREA_STYLE ('',( #2531 ) ) ;
#3196 = AXIS2_PLACEMENT_3D ( 'NONE', #966, #336, #7739 ) ;
#3197 = CARTESIAN_POINT ( 'NONE',  ( -3.200000000000008171, 0.000000000000000000, 0.000000000000000000 ) ) ;
#3198 = EDGE_LOOP ( 'NONE', ( #4699, #49, #3545, #6273 ) ) ;
#3199 =( REPRESENTATION_RELATIONSHIP ('NONE','NONE', #1229, #420 ) REPRESENTATION_RELATIONSHIP_WITH_TRANSFORMATION ( #3530 )SHAPE_REPRESENTATION_RELATIONSHIP( ) );
#3200 = ORIENTED_EDGE ( 'NONE', *, *, #82, .F. ) ;
#3201 = CARTESIAN_POINT ( 'NONE',  ( 26.26644452187122170, -80.83980388508783221, 0.000000000000000000 ) ) ;
#3202 = DIRECTION ( 'NONE',  ( 0.000000000000000000, 0.000000000000000000, 1.000000000000000000 ) ) ;
#3203 = CYLINDRICAL_SURFACE ( 'NONE', #6281, 29.99999999999999289 ) ;
#3204 = TOROIDAL_SURFACE ( 'NONE', #4458, 37.19999999999999574, 0.3000000000000007661 ) ;
#3205 = CYLINDRICAL_SURFACE ( 'NONE', #5829, 5.249999999999992006 ) ;
#3206 = ORIENTED_EDGE ( 'NONE', *, *, #707, .T. ) ;
#3207 = EDGE_CURVE ( 'NONE', #2604, #7338, #4368, .T. ) ;
#3208 = VECTOR ( 'NONE', #5506, 1000.000000000000000 ) ;
#3209 = CARTESIAN_POINT ( 'NONE',  ( -0.6527133886630326343, 8.860760056385741379, -0.4969600502617543270 ) ) ;
#3210 = DIRECTION ( 'NONE',  ( 1.000000000000000000, 0.000000000000000000, 0.000000000000000000 ) ) ;
#3211 = LINE ( 'NONE', #950, #3883 ) ;
#3212 = EDGE_CURVE ( 'NONE', #7629, #1985, #242, .T. ) ;
#3213 = DIRECTION ( 'NONE',  ( 0.000000000000000000, 0.000000000000000000, -1.000000000000000000 ) ) ;
#3214 = CIRCLE ( 'NONE', #7612, 32.25000000000000000 ) ;
#3215 = ORIENTED_EDGE ( 'NONE', *, *, #1184, .T. ) ;
#3216 = PRESENTATION_LAYER_ASSIGNMENT (  '', '', ( #2840 ) ) ;
#3217 = DIRECTION ( 'NONE',  ( 1.000000000000000000, 0.000000000000000000, 0.000000000000000000 ) ) ;
#3218 = FACE_OUTER_BOUND ( 'NONE', #2768, .T. ) ;
#3219 = EDGE_CURVE ( 'NONE', #1212, #3662, #3971, .T. ) ;
#3220 = AXIS2_PLACEMENT_3D ( 'NONE', #654, #5431, #7168 ) ;
#3221 = CLOSED_SHELL ( 'NONE', ( #4175, #3792, #5574, #3125, #409, #6690, #4140, #1492, #6157, #7493, #1728, #3602, #5232, #4864 ) ) ;
#3222 = DIRECTION ( 'NONE',  ( 0.000000000000000000, 0.000000000000000000, 1.000000000000000000 ) ) ;
#3223 = LINE ( 'NONE', #1515, #4499 ) ;
#3224 = CARTESIAN_POINT ( 'NONE',  ( -4.857225732735059864E-13, 239.9963296805738082, 14.70000000000000462 ) ) ;
#3225 = PRODUCT_DEFINITION_SHAPE ( 'NONE', 'NONE',  #6722 ) ;
#3226 = EDGE_CURVE ( 'NONE', #3377, #5317, #1633, .T. ) ;
#3227 = CARTESIAN_POINT ( 'NONE',  ( 0.6527133886630215320, -8.860760056385755590, -4.203039949738235137 ) ) ;
#3228 = FACE_OUTER_BOUND ( 'NONE', #6706, .T. ) ;
#3229 = ORIENTED_EDGE ( 'NONE', *, *, #5631, .F. ) ;
#3230 = ORIENTED_EDGE ( 'NONE', *, *, #6924, .F. ) ;
#3231 = VERTEX_POINT ( 'NONE', #5154 ) ;
#3232 = EDGE_CURVE ( 'NONE', #5609, #6843, #2774, .T. ) ;
#3233 = FACE_OUTER_BOUND ( 'NONE', #4739, .T. ) ;
#3234 = CARTESIAN_POINT ( 'NONE',  ( 0.000000000000000000, 0.000000000000000000, 13.00000000000001066 ) ) ;
#3235 = CIRCLE ( 'NONE', #3704, 35.25000000000000000 ) ;
#3236 = CARTESIAN_POINT ( 'NONE',  ( 89.90381056766652534, -74.99999999999882050, 10.00000000000000000 ) ) ;
#3237 = EDGE_CURVE ( 'NONE', #7233, #6072, #4487, .T. ) ;
#3238 = ORIENTED_EDGE ( 'NONE', *, *, #7448, .F. ) ;
#3239 = AXIS2_PLACEMENT_3D ( 'NONE', #7348, #3565, #5975 ) ;
#3240 = EDGE_LOOP ( 'NONE', ( #853, #5036, #2416, #2452, #4343, #2949, #5078, #7734, #1440, #2916, #33, #5444, #3482, #4229, #255 ) ) ;
#3241 = DIRECTION ( 'NONE',  ( 0.000000000000000000, 0.000000000000000000, 1.000000000000000000 ) ) ;
#3242 = LINE ( 'NONE', #5828, #4768 ) ;
#3243 = APPLICATION_CONTEXT ( 'automotive_design' ) ;
#3244 = DIRECTION ( 'NONE',  ( -0.000000000000000000, -0.000000000000000000, 1.000000000000000000 ) ) ;
#3245 = ORIENTED_EDGE ( 'NONE', *, *, #1276, .F. ) ;
#3246 = AXIS2_PLACEMENT_3D ( 'NONE', #2288, #1088, #3499 ) ;
#3247 = DIRECTION ( 'NONE',  ( 0.000000000000000000, 0.000000000000000000, 1.000000000000000000 ) ) ;
#3248 = FACE_OUTER_BOUND ( 'NONE', #1409, .T. ) ;
#3249 = CARTESIAN_POINT ( 'NONE',  ( 3.200000000000007727, 0.000000000000000000, 0.000000000000000000 ) ) ;
#3250 = AXIS2_PLACEMENT_3D ( 'NONE', #1676, #7706, #4632 ) ;
#3251 = CARTESIAN_POINT ( 'NONE',  ( -3.199999999999994404, 0.000000000000000000, 0.000000000000000000 ) ) ;
#3252 = ORIENTED_EDGE ( 'NONE', *, *, #2928, .F. ) ;
#3253 = DIRECTION ( 'NONE',  ( -2.485795968188197231E-17, 1.883273162252411239E-17, 1.000000000000000000 ) ) ;
#3254 = AXIS2_PLACEMENT_3D ( 'NONE', #4930, #4341, #1264 ) ;
#3255 = DIRECTION ( 'NONE',  ( 1.000000000000000000, 0.000000000000000000, 0.000000000000000000 ) ) ;
#3256 = DIRECTION ( 'NONE',  ( 0.000000000000000000, 0.000000000000000000, -1.000000000000000000 ) ) ;
#3257 = LINE ( 'NONE', #6372, #3992 ) ;
#3258 = PRODUCT_CONTEXT ( 'NONE', #4595, 'mechanical' ) ;
#3259 = AXIS2_PLACEMENT_3D ( 'NONE', #1281, #4279, #4795 ) ;
#3260 = DIRECTION ( 'NONE',  ( -0.000000000000000000, -0.000000000000000000, 1.000000000000000000 ) ) ;
#3261 = EDGE_CURVE ( 'NONE', #4264, #816, #501, .T. ) ;
#3262 = LINE ( 'NONE', #2047, #6922 ) ;
#3263 = ORIENTED_EDGE ( 'NONE', *, *, #6406, .T. ) ;
#3264 = EDGE_CURVE ( 'NONE', #6807, #5454, #7444, .T. ) ;
#3265 = ORIENTED_EDGE ( 'NONE', *, *, #988, .F. ) ;
#3266 = EDGE_CURVE ( 'NONE', #1601, #2088, #7186, .T. ) ;
#3267 = ORIENTED_EDGE ( 'NONE', *, *, #2553, .T. ) ;
#3268 = AXIS2_PLACEMENT_3D ( 'NONE', #6132, #5797, #6318 ) ;
#3269 = EDGE_CURVE ( 'NONE', #7689, #3301, #4933, .T. ) ;
#3270 = EDGE_LOOP ( 'NONE', ( #2132, #3416, #2007, #3573 ) ) ;
#3271 = DIRECTION ( 'NONE',  ( -0.000000000000000000, -0.000000000000000000, 1.000000000000000000 ) ) ;
#3272 = DIRECTION ( 'NONE',  ( -0.000000000000000000, -0.000000000000000000, 1.000000000000000000 ) ) ;
#3273 = SHAPE_REPRESENTATION_RELATIONSHIP ( 'NONE' , 'NONE' ,  #7725, #5288 ) ;
#3274 = CARTESIAN_POINT ( 'NONE',  ( 10.16320117273318679, -26.62629042736811869, -122.9999999999999716 ) ) ;
#3275 = AXIS2_PLACEMENT_3D ( 'NONE', #6853, #3856, #7437 ) ;
#3276 = ORIENTED_EDGE ( 'NONE', *, *, #2314, .F. ) ;
#3277 = VERTEX_POINT ( 'NONE', #3346 ) ;
#3278 = MECHANICAL_DESIGN_GEOMETRIC_PRESENTATION_REPRESENTATION (  '', ( #3027 ), #7426 ) ;
#3279 = FACE_OUTER_BOUND ( 'NONE', #4920, .T. ) ;
#3280 = FACE_OUTER_BOUND ( 'NONE', #2203, .T. ) ;
#3281 = DIRECTION ( 'NONE',  ( 0.000000000000000000, 0.000000000000000000, 1.000000000000000000 ) ) ;
#3282 = CARTESIAN_POINT ( 'NONE',  ( -3.499999999999996003, 0.000000000000000000, 0.000000000000000000 ) ) ;
#3283 = ORIENTED_EDGE ( 'NONE', *, *, #176, .T. ) ;
#3284 = AXIS2_PLACEMENT_3D ( 'NONE', #1106, #2971, #1146 ) ;
#3285 = PRODUCT_DEFINITION_SHAPE ( 'NONE', 'NONE',  #7777 ) ;
#3286 = CARTESIAN_POINT ( 'NONE',  ( -119.9981648402875578, 207.8429183184017859, -50.00000000000000000 ) ) ;
#3287 = CYLINDRICAL_SURFACE ( 'NONE', #6730, 150.0000000000000568 ) ;
#3288 = CARTESIAN_POINT ( 'NONE',  ( 279.9963296805736945, -6.783120157456498832E-12, 10.00000000000000000 ) ) ;
#3289 = DIRECTION ( 'NONE',  ( 1.000000000000000000, 0.000000000000000000, 0.000000000000000000 ) ) ;
#3290 = VERTEX_POINT ( 'NONE', #4526 ) ;
#3291 = AXIS2_PLACEMENT_3D ( 'NONE', #6229, #2094, #6342 ) ;
#3292 = DIRECTION ( 'NONE',  ( 0.000000000000000000, 1.000000000000000000, 0.000000000000000000 ) ) ;
#3293 = DIRECTION ( 'NONE',  ( -0.000000000000000000, -0.000000000000000000, -1.000000000000000000 ) ) ;
#3294 = CYLINDRICAL_SURFACE ( 'NONE', #4080, 29.99999999999999289 ) ;
#3295 = CYLINDRICAL_SURFACE ( 'NONE', #2632, 35.00000000000000711 ) ;
#3296 = CARTESIAN_POINT ( 'NONE',  ( -64.59444452187068464, 49.96174644486002592, -65.00000000000000000 ) ) ;
#3297 = APPLICATION_PROTOCOL_DEFINITION ( 'draft international standard', 'automotive_design', 1998, #2948 ) ;
#3298 = CARTESIAN_POINT ( 'NONE',  ( 5.249999999999482192, 239.9963296805737230, -50.00000000000000000 ) ) ;
#3299 = VERTEX_POINT ( 'NONE', #2642 ) ;
#3300 = ORIENTED_EDGE ( 'NONE', *, *, #7014, .F. ) ;
#3301 = VERTEX_POINT ( 'NONE', #338 ) ;
#3302 = ORIENTED_EDGE ( 'NONE', *, *, #2507, .F. ) ;
#3303 = CYLINDRICAL_SURFACE ( 'NONE', #4976, 35.00000000000000711 ) ;
#3304 = CARTESIAN_POINT ( 'NONE',  ( -68.76644452187068168, 49.96174644486002592, -40.00000000000000000 ) ) ;
#3305 = DIRECTION ( 'NONE',  ( -0.000000000000000000, -0.000000000000000000, -1.000000000000000000 ) ) ;
#3306 = FILL_AREA_STYLE_COLOUR ( '', #5099 ) ;
#3307 = DIRECTION ( 'NONE',  ( 3.081487911019577365E-33, -2.775557561562891967E-17, -1.000000000000000000 ) ) ;
#3308 = CONICAL_SURFACE ( 'NONE', #906, 5.000000000000000888, 0.9599310885968824758 ) ;
#3309 = EDGE_CURVE ( 'NONE', #294, #989, #2172, .T. ) ;
#3310 = ORIENTED_EDGE ( 'NONE', *, *, #2324, .F. ) ;
#3311 = ORIENTED_EDGE ( 'NONE', *, *, #3974, .T. ) ;
#3312 = VERTEX_POINT ( 'NONE', #1449 ) ;
#3313 = AXIS2_PLACEMENT_3D ( 'NONE', #2973, #2429, #6710 ) ;
#3314 = AXIS2_PLACEMENT_3D ( 'NONE', #5083, #7380, #2027 ) ;
#3315 = FACE_OUTER_BOUND ( 'NONE', #6561, .T. ) ;
#3316 = ADVANCED_FACE ( 'NONE', ( #930 ), #892, .F. ) ;
#3317 = CARTESIAN_POINT ( 'NONE',  ( 0.000000000000000000, 1.484218055610305731, -3.000000000000000000 ) ) ;
#3318 = CARTESIAN_POINT ( 'NONE',  ( 1.313474075707211197, 8.479269695850863542, -0.3167204509598410267 ) ) ;
#3319 = CIRCLE ( 'NONE', #546, 28.49999999999999645 ) ;
#3320 = VERTEX_POINT ( 'NONE', #6972 ) ;
#3321 = DIRECTION ( 'NONE',  ( 0.01999999999999999001, 0.9997999799959990108, 0.000000000000000000 ) ) ;
#3322 = DIRECTION ( 'NONE',  ( -0.000000000000000000, -0.000000000000000000, 1.000000000000000000 ) ) ;
#3323 = CIRCLE ( 'NONE', #415, 29.99999999999999289 ) ;
#3324 = CARTESIAN_POINT ( 'NONE',  ( 11.50644898236017433, -35.69105814929478981, 0.000000000000000000 ) ) ;
#3325 = CARTESIAN_POINT ( 'NONE',  ( 129.9038105676665396, -74.99999999999882050, 0.000000000000000000 ) ) ;
#3326 = ADVANCED_FACE ( 'NONE', ( #968 ), #3385, .F. ) ;
#3327 = ORIENTED_EDGE ( 'NONE', *, *, #757, .T. ) ;
#3328 = CIRCLE ( 'NONE', #1822, 40.00000000000000711 ) ;
#3329 = VECTOR ( 'NONE', #4666, 1000.000000000000000 ) ;
#3330 = DIRECTION ( 'NONE',  ( 0.000000000000000000, 0.000000000000000000, 1.000000000000000000 ) ) ;
#3331 = DIRECTION ( 'NONE',  ( 0.000000000000000000, 0.000000000000000000, 1.000000000000000000 ) ) ;
#3332 = CARTESIAN_POINT ( 'NONE',  ( -8.000000000000000000, 0.000000000000000000, 0.000000000000000000 ) ) ;
#3333 = LINE ( 'NONE', #6446, #3016 ) ;
#3334 = DIRECTION ( 'NONE',  ( 1.000000000000000000, 0.000000000000000000, 0.000000000000000000 ) ) ;
#3335 = CONTEXT_DEPENDENT_SHAPE_REPRESENTATION ( #1420, #4410 ) ;
#3336 = CIRCLE ( 'NONE', #3591, 5.249999999999977796 ) ;
#3337 = AXIS2_PLACEMENT_3D ( 'NONE', #4154, #6122, #1114 ) ;
#3338 = CARTESIAN_POINT ( 'NONE',  ( 2.309976723937607890, -7.903938623646878270, -4.569346954796185578 ) ) ;
#3339 = ORIENTED_EDGE ( 'NONE', *, *, #7693, .F. ) ;
#3340 = ORIENTED_EDGE ( 'NONE', *, *, #6542, .T. ) ;
#3341 = ORIENTED_EDGE ( 'NONE', *, *, #3168, .T. ) ;
#3342 = ORIENTED_EDGE ( 'NONE', *, *, #5880, .T. ) ;
#3343 = DIRECTION ( 'NONE',  ( 1.000000000000000000, 0.000000000000000000, -0.000000000000000000 ) ) ;
#3344 =( REPRESENTATION_RELATIONSHIP ('NONE','NONE', #1229, #1433 ) REPRESENTATION_RELATIONSHIP_WITH_TRANSFORMATION ( #3999 )SHAPE_REPRESENTATION_RELATIONSHIP( ) );
#3345 = CARTESIAN_POINT ( 'NONE',  ( 2.503857664561936813E-16, -9.237604307034025908, -4.700000000000000178 ) ) ;
#3346 = CARTESIAN_POINT ( 'NONE',  ( 2.583028308771596837, 28.38270538120150377, 10.00000000000000000 ) ) ;
#3347 = CARTESIAN_POINT ( 'NONE',  ( 0.000000000000000000, 0.000000000000000000, 0.000000000000000000 ) ) ;
#3348 = CYLINDRICAL_SURFACE ( 'NONE', #7601, 4.999999999999990230 ) ;
#3349 = PRODUCT_RELATED_PRODUCT_CATEGORY ( 'part', '', ( #6 ) ) ;
#3350 = VERTEX_POINT ( 'NONE', #378 ) ;
#3351 = ORIENTED_EDGE ( 'NONE', *, *, #5352, .F. ) ;
#3352 = ORIENTED_EDGE ( 'NONE', *, *, #7040, .T. ) ;
#3353 = CARTESIAN_POINT ( 'NONE',  ( -68.76644452187068168, 49.96174644486002592, 0.000000000000000000 ) ) ;
#3354 = DIRECTION ( 'NONE',  ( -0.000000000000000000, -0.000000000000000000, 1.000000000000000000 ) ) ;
#3355 = CIRCLE ( 'NONE', #324, 0.3000000000000016542 ) ;
#3356 = CARTESIAN_POINT ( 'NONE',  ( -39.64284999284934941, 144.6666666666667140, 5.000000000000000000 ) ) ;
#3357 = EDGE_CURVE ( 'NONE', #406, #1868, #2901, .T. ) ;
#3358 = ORIENTED_EDGE ( 'NONE', *, *, #2651, .F. ) ;
#3359 = ADVANCED_FACE ( 'NONE', ( #1489 ), #3159, .T. ) ;
#3360 = ADVANCED_FACE ( 'NONE', ( #2797 ), #4604, .T. ) ;
#3361 = AXIS2_PLACEMENT_3D ( 'NONE', #1394, #2702, #5101 ) ;
#3362 = EDGE_CURVE ( 'NONE', #5940, #599, #2717, .T. ) ;
#3363 = DIRECTION ( 'NONE',  ( 1.000000000000000000, 0.000000000000000000, 0.000000000000000000 ) ) ;
#3364 = CARTESIAN_POINT ( 'NONE',  ( 10.00000000000000000, 28.28427124746190202, 0.000000000000000000 ) ) ;
#3365 = DIRECTION ( 'NONE',  ( 1.000000000000000000, 0.000000000000000000, 0.000000000000000000 ) ) ;
#3366 = CARTESIAN_POINT ( 'NONE',  ( -7.347286611336972584, -4.995646404165285936, -4.203039949738244019 ) ) ;
#3367 = EDGE_LOOP ( 'NONE', ( #7045, #5697, #2138, #2968 ) ) ;
#3368 = EDGE_CURVE ( 'NONE', #5511, #2491, #5038, .T. ) ;
#3369 = CIRCLE ( 'NONE', #4879, 37.50000000000000000 ) ;
#3370 = DIRECTION ( 'NONE',  ( 0.000000000000000000, 0.000000000000000000, 1.000000000000000000 ) ) ;
#3371 = CARTESIAN_POINT ( 'NONE',  ( -20.63749999999999574, 0.000000000000000000, 0.000000000000000000 ) ) ;
#3372 = CIRCLE ( 'NONE', #3631, 4.171999999999995268 ) ;
#3373 = DIRECTION ( 'NONE',  ( 1.000000000000000000, 0.000000000000000000, 0.000000000000000000 ) ) ;
#3374 = CARTESIAN_POINT ( 'NONE',  ( -145.1064334105733451, -38.00161816111073421, 0.000000000000000000 ) ) ;
#3375 = DIRECTION ( 'NONE',  ( 0.000000000000000000, 0.000000000000000000, 1.000000000000000000 ) ) ;
#3376 = CARTESIAN_POINT ( 'NONE',  ( -10.00000000000000000, 42.00000000000000000, 0.000000000000000000 ) ) ;
#3377 = VERTEX_POINT ( 'NONE', #1623 ) ;
#3378 = VERTEX_POINT ( 'NONE', #7028 ) ;
#3379 = VECTOR ( 'NONE', #2698, 1000.000000000000000 ) ;
#3380 = VERTEX_POINT ( 'NONE', #6596 ) ;
#3381 = CARTESIAN_POINT ( 'NONE',  ( 10.00000000000000000, 28.28427124746190202, 10.00000000000000000 ) ) ;
#3382 = CARTESIAN_POINT ( 'NONE',  ( 39.64284999284934230, -144.6666666666667140, 0.000000000000000000 ) ) ;
#3383 = CIRCLE ( 'NONE', #5403, 0.3000000000000016542 ) ;
#3384 = DIRECTION ( 'NONE',  ( 0.000000000000000000, 0.000000000000000000, 1.000000000000000000 ) ) ;
#3385 = CYLINDRICAL_SURFACE ( 'NONE', #3905, 37.49999999999997868 ) ;
#3386 = SURFACE_STYLE_FILL_AREA ( #456 ) ;
#3387 = VECTOR ( 'NONE', #4419, 1000.000000000000000 ) ;
#3388 = CARTESIAN_POINT ( 'NONE',  ( 31.51644452187122525, -80.83980388508783221, 10.00000000000000000 ) ) ;
#3389 = ORIENTED_EDGE ( 'NONE', *, *, #3030, .T. ) ;
#3390 = CIRCLE ( 'NONE', #4391, 5.249999999999976907 ) ;
#3391 = VERTEX_POINT ( 'NONE', #2386 ) ;
#3392 = VERTEX_POINT ( 'NONE', #5925 ) ;
#3393 = CARTESIAN_POINT ( 'NONE',  ( 0.000000000000000000, 0.000000000000000000, 2.573333333333333695 ) ) ;
#3394 = AXIS2_PLACEMENT_3D ( 'NONE', #2360, #5978, #4862 ) ;
#3395 = DIRECTION ( 'NONE',  ( -0.000000000000000000, -0.000000000000000000, 1.000000000000000000 ) ) ;
#3396 = CARTESIAN_POINT ( 'NONE',  ( 0.000000000000000000, 0.000000000000000000, 0.000000000000000000 ) ) ;
#3397 = EDGE_LOOP ( 'NONE', ( #4682, #116, #2736, #7347 ) ) ;
#3398 = EDGE_CURVE ( 'NONE', #1025, #1540, #1021, .T. ) ;
#3399 = DIRECTION ( 'NONE',  ( 0.000000000000000000, 0.000000000000000000, 1.000000000000000000 ) ) ;
#3400 = DIRECTION ( 'NONE',  ( 0.5000000000000006661, -0.8660254037844382635, 0.000000000000000000 ) ) ;
#3401 = LINE ( 'NONE', #7189, #7030 ) ;
#3402=STYLED_ITEM('',(#7837),#3183);
#3403 = EDGE_CURVE ( 'NONE', #3181, #2263, #4408, .T. ) ;
#3404 = CYLINDRICAL_SURFACE ( 'NONE', #4934, 32.25000000000000000 ) ;
#3405 = ORIENTED_EDGE ( 'NONE', *, *, #1443, .F. ) ;
#3406 = EDGE_CURVE ( 'NONE', #5637, #4200, #6557, .T. ) ;
#3407 = FACE_OUTER_BOUND ( 'NONE', #5112, .T. ) ;
#3408 = AXIS2_PLACEMENT_3D ( 'NONE', #748, #5485, #4928 ) ;
#3409 = CYLINDRICAL_SURFACE ( 'NONE', #2208, 37.50000000000000000 ) ;
#3410 = DIRECTION ( 'NONE',  ( -0.000000000000000000, -0.000000000000000000, -1.000000000000000000 ) ) ;
#3411 = CARTESIAN_POINT ( 'NONE',  ( 0.000000000000000000, 0.000000000000000000, 576.0908266162076643 ) ) ;
#3412 = ADVANCED_FACE ( 'NONE', ( #7145 ), #4026, .F. ) ;
#3413 = DIRECTION ( 'NONE',  ( 5.551115123125782702E-17, -0.000000000000000000, 1.000000000000000000 ) ) ;
#3414 = TOROIDAL_SURFACE ( 'NONE', #5045, 33.75000000000000000, 2.250000000000000444 ) ;
#3415 = ORIENTED_EDGE ( 'NONE', *, *, #3563, .T. ) ;
#3416 = ORIENTED_EDGE ( 'NONE', *, *, #5302, .T. ) ;
#3417 = ORIENTED_EDGE ( 'NONE', *, *, #2400, .F. ) ;
#3418 = DIRECTION ( 'NONE',  ( 0.000000000000000000, 0.000000000000000000, 1.000000000000000000 ) ) ;
#3419 = CARTESIAN_POINT ( 'NONE',  ( 5.690023276062393442, 5.952467836904152598, -0.1306530452038090484 ) ) ;
#3420 = DIRECTION ( 'NONE',  ( 1.000000000000000000, 0.000000000000000000, 0.000000000000000000 ) ) ;
#3421 = DIRECTION ( 'NONE',  ( 0.000000000000000000, 0.000000000000000000, 1.000000000000000000 ) ) ;
#3422 = CARTESIAN_POINT ( 'NONE',  ( -8.000000000000000000, -4.618802153517013842, -3.985468820183668104 ) ) ;
#3423 = EDGE_CURVE ( 'NONE', #589, #3903, #5841, .T. ) ;
#3424 = VERTEX_POINT ( 'NONE', #2347 ) ;
#3425 = EDGE_LOOP ( 'NONE', ( #7709, #6522, #933, #107 ) ) ;
#3426 = ORIENTED_EDGE ( 'NONE', *, *, #6398, .F. ) ;
#3427 = CARTESIAN_POINT ( 'NONE',  ( 79.75000000000000000, 9.726431976288768917E-13, 10.00000000000000000 ) ) ;
#3428 = CIRCLE ( 'NONE', #4182, 150.0000000000000568 ) ;
#3429 = DIRECTION ( 'NONE',  ( 0.000000000000000000, 0.000000000000000000, 1.000000000000000000 ) ) ;
#3430 = CARTESIAN_POINT ( 'NONE',  ( -5.238334947888650284, -36.57199107895616663, 0.000000000000000000 ) ) ;
#3431 = VERTEX_POINT ( 'NONE', #6437 ) ;
#3432 = CIRCLE ( 'NONE', #158, 35.97500000000000142 ) ;
#3433 = ORIENTED_EDGE ( 'NONE', *, *, #610, .T. ) ;
#3434 = DIRECTION ( 'NONE',  ( 1.000000000000000000, 0.000000000000000000, 0.000000000000000000 ) ) ;
#3435 = CARTESIAN_POINT ( 'NONE',  ( 32.49999999999997158, 3.980102097228894682E-15, -119.9999999999999858 ) ) ;
#3436 = DIRECTION ( 'NONE',  ( 0.000000000000000000, 0.000000000000000000, 1.000000000000000000 ) ) ;
#3437 = AXIS2_PLACEMENT_3D ( 'NONE', #1232, #3644, #1874 ) ;
#3438 = CARTESIAN_POINT ( 'NONE',  ( 0.000000000000000000, 0.000000000000000000, -4.674599999999997202 ) ) ;
#3439 = ORIENTED_EDGE ( 'NONE', *, *, #394, .T. ) ;
#3440 = EDGE_CURVE ( 'NONE', #1095, #5377, #2538, .T. ) ;
#3441 = ORIENTED_EDGE ( 'NONE', *, *, #705, .F. ) ;
#3442 = CARTESIAN_POINT ( 'NONE',  ( 10.00000000000000000, 41.99999999999999289, -60.00000000000000711 ) ) ;
#3443 = VECTOR ( 'NONE', #5516, 1000.000000000000000 ) ;
#3444 = FILL_AREA_STYLE_COLOUR ( '', #6001 ) ;
#3445 = FACE_OUTER_BOUND ( 'NONE', #4411, .T. ) ;
#3446 = DIRECTION ( 'NONE',  ( -0.09063257223759992043, -0.9958843993404034034, 0.000000000000000000 ) ) ;
#3447 = CARTESIAN_POINT ( 'NONE',  ( -2.750000000000000000, -33.63777638310832430, -3.000000000000000000 ) ) ;
#3448 = CONTEXT_DEPENDENT_SHAPE_REPRESENTATION ( #7564, #1321 ) ;
#3449 = CARTESIAN_POINT ( 'NONE',  ( 350.0000000000000000, -300.0000000000000000, -1041.954445729288636 ) ) ;
#3450 = CONICAL_SURFACE ( 'NONE', #4834, 4.999999999999990230, 0.7853981633974482790 ) ;
#3451 = EDGE_LOOP ( 'NONE', ( #6176, #2802 ) ) ;
#3452 = AXIS2_PLACEMENT_3D ( 'NONE', #356, #5686, #2696 ) ;
#3453 = ORIENTED_EDGE ( 'NONE', *, *, #5920, .F. ) ;
#3454 = ORIENTED_EDGE ( 'NONE', *, *, #6025, .F. ) ;
#3455 = ADVANCED_FACE ( 'NONE', ( #1753 ), #7188, .F. ) ;
#3456 = CARTESIAN_POINT ( 'NONE',  ( -1.310872448937999035, 8.480771745766400471, -4.382649155111345785 ) ) ;
#3457 = AXIS2_PLACEMENT_3D ( 'NONE', #6731, #3693, #1922 ) ;
#3458 = CIRCLE ( 'NONE', #3337, 0.3000000000000016542 ) ;
#3459 = EDGE_CURVE ( 'NONE', #3634, #4724, #1901, .T. ) ;
#3460 = FACE_OUTER_BOUND ( 'NONE', #6881, .T. ) ;
#3461 = CYLINDRICAL_SURFACE ( 'NONE', #3246, 35.25000000000000000 ) ;
#3462 =( LENGTH_UNIT ( ) NAMED_UNIT ( * ) SI_UNIT ( .MILLI., .METRE. ) );
#3463 = DIRECTION ( 'NONE',  ( -0.000000000000000000, -0.000000000000000000, 1.000000000000000000 ) ) ;
#3464 = CONICAL_SURFACE ( 'NONE', #4846, 37.49999999999997868, 1.029744258676654090 ) ;
#3465 = ORIENTED_EDGE ( 'NONE', *, *, #5863, .F. ) ;
#3466 = ADVANCED_FACE ( 'NONE', ( #6590 ), #7695, .T. ) ;
#3467 = PRESENTATION_LAYER_ASSIGNMENT (  '', '', ( #6867 ) ) ;
#3468 = EDGE_LOOP ( 'NONE', ( #2603, #6699, #6821, #3583 ) ) ;
#3469 = VERTEX_POINT ( 'NONE', #4659 ) ;
#3470 = CARTESIAN_POINT ( 'NONE',  ( -8.000000000000000000, 4.618802153517013842, -3.985468820183668104 ) ) ;
#3471 = EDGE_CURVE ( 'NONE', #1710, #4364, #2417, .T. ) ;
#3472 = AXIS2_PLACEMENT_3D ( 'NONE', #4797, #1166, #1127 ) ;
#3473 = CARTESIAN_POINT ( 'NONE',  ( 21.01644452187122170, -80.83980388508783221, 10.00000000000000000 ) ) ;
#3474 = CARTESIAN_POINT ( 'NONE',  ( 0.000000000000000000, 0.000000000000000000, 0.000000000000000000 ) ) ;
#3475 = ORIENTED_EDGE ( 'NONE', *, *, #7750, .T. ) ;
#3476 = MECHANICAL_DESIGN_GEOMETRIC_PRESENTATION_REPRESENTATION (  '', ( #3729 ), #1977 ) ;
#3477 = DIRECTION ( 'NONE',  ( 1.000000000000000000, 0.000000000000000000, 0.000000000000000000 ) ) ;
#3478 = FACE_OUTER_BOUND ( 'NONE', #2076, .T. ) ;
#3479 = MECHANICAL_DESIGN_GEOMETRIC_PRESENTATION_REPRESENTATION (  '', ( #2978 ), #1073 ) ;
#3480 = DIRECTION ( 'NONE',  ( 1.000000000000000000, 0.000000000000000000, 0.000000000000000000 ) ) ;
#3481 = CARTESIAN_POINT ( 'NONE',  ( 9.090232026328989079, -27.01143612819398143, -122.9999999999999716 ) ) ;
#3482 = ORIENTED_EDGE ( 'NONE', *, *, #938, .T. ) ;
#3483 = ORIENTED_EDGE ( 'NONE', *, *, #1027, .T. ) ;
#3484 = AXIS2_PLACEMENT_3D ( 'NONE', #1065, #6361, #1662 ) ;
#3485 = DIRECTION ( 'NONE',  ( 0.000000000000000000, 0.000000000000000000, 1.000000000000000000 ) ) ;
#3486 = FACE_OUTER_BOUND ( 'NONE', #4481, .T. ) ;
#3487 = CARTESIAN_POINT ( 'NONE',  ( -8.000000000000000000, -0.7805016046291017862, -4.700000000000000178 ) ) ;
#3488 = DIRECTION ( 'NONE',  ( 0.000000000000000000, 0.000000000000000000, 1.000000000000000000 ) ) ;
#3489 = DIRECTION ( 'NONE',  ( 1.000000000000000000, 0.000000000000000000, 0.000000000000000000 ) ) ;
#3490 = CARTESIAN_POINT ( 'NONE',  ( 29.99999999999999289, 0.000000000000000000, 13.00000000000001066 ) ) ;
#3491 = ORIENTED_EDGE ( 'NONE', *, *, #6400, .F. ) ;
#3492 =( REPRESENTATION_RELATIONSHIP ('NONE','NONE', #1229, #2306 ) REPRESENTATION_RELATIONSHIP_WITH_TRANSFORMATION ( #3647 )SHAPE_REPRESENTATION_RELATIONSHIP( ) );
#3493 = ORIENTED_EDGE ( 'NONE', *, *, #7127, .F. ) ;
#3494 = ORIENTED_EDGE ( 'NONE', *, *, #4523, .T. ) ;
#3495 = CIRCLE ( 'NONE', #2376, 31.52499999999999858 ) ;
#3496 = DIRECTION ( 'NONE',  ( 1.000000000000000000, -2.398081733190337496E-14, 0.000000000000000000 ) ) ;
#3497 = EDGE_CURVE ( 'NONE', #2604, #6348, #3535, .T. ) ;
#3498 = DIRECTION ( 'NONE',  ( -0.9914448613738101601, -0.1305261922200541547, 0.000000000000000000 ) ) ;
#3499 = DIRECTION ( 'NONE',  ( 0.000000000000000000, 0.000000000000000000, -1.000000000000000000 ) ) ;
#3500 = DIRECTION ( 'NONE',  ( 0.000000000000000000, 0.000000000000000000, 1.000000000000000000 ) ) ;
#3501 = CARTESIAN_POINT ( 'NONE',  ( -68.76644452187068168, 49.96174644486002592, 0.000000000000000000 ) ) ;
#3502 = DIRECTION ( 'NONE',  ( -1.000000000000000000, 0.000000000000000000, 0.000000000000000000 ) ) ;
#3503 = EDGE_CURVE ( 'NONE', #6073, #2129, #4538, .T. ) ;
#3504 = ADVANCED_FACE ( 'NONE', ( #1066, #3478 ), #1792, .T. ) ;
#3505 = CIRCLE ( 'NONE', #850, 7.999999999999998224 ) ;
#3506 = VERTEX_POINT ( 'NONE', #2892 ) ;
#3507 = ADVANCED_FACE ( 'NONE', ( #4184 ), #5039, .T. ) ;
#3508 = ORIENTED_EDGE ( 'NONE', *, *, #2752, .F. ) ;
#3509 = VERTEX_POINT ( 'NONE', #7614 ) ;
#3510 = VECTOR ( 'NONE', #5926, 1000.000000000000000 ) ;
#3511 = CARTESIAN_POINT ( 'NONE',  ( 129.9038105676649764, 75.00000000000153477, 0.000000000000000000 ) ) ;
#3512 = DIRECTION ( 'NONE',  ( -0.000000000000000000, -0.000000000000000000, 1.000000000000000000 ) ) ;
#3513 = CARTESIAN_POINT ( 'NONE',  ( 26.82422866010495710, 9.628642520646586433, -122.9999999999999716 ) ) ;
#3514 = ADVANCED_FACE ( 'NONE', ( #4622 ), #4852, .T. ) ;
#3515 = VECTOR ( 'NONE', #6925, 1000.000000000000000 ) ;
#3516 = ORIENTED_EDGE ( 'NONE', *, *, #6493, .F. ) ;
#3517 = VERTEX_POINT ( 'NONE', #7264 ) ;
#3518 = DIRECTION ( 'NONE',  ( 0.000000000000000000, 0.000000000000000000, 1.000000000000000000 ) ) ;
#3519 = DIRECTION ( 'NONE',  ( -0.000000000000000000, 1.000000000000000000, 0.000000000000000000 ) ) ;
#3520 = LINE ( 'NONE', #4660, #3510 ) ;
#3521 = CARTESIAN_POINT ( 'NONE',  ( -4.680456609903975718, -6.535341423375596648, -4.683111142572228047 ) ) ;
#3522 = ORIENTED_EDGE ( 'NONE', *, *, #3025, .T. ) ;
#3523 = EDGE_LOOP ( 'NONE', ( #6573, #6857, #6768 ) ) ;
#3524 = FACE_BOUND ( 'NONE', #3826, .T. ) ;
#3525 = DIRECTION ( 'NONE',  ( 1.000000000000000000, 0.000000000000000000, 0.000000000000000000 ) ) ;
#3526 = CARTESIAN_POINT ( 'NONE',  ( 3.499999999999996003, 0.000000000000000000, -35.25000000000000000 ) ) ;
#3527 =( LENGTH_UNIT ( ) NAMED_UNIT ( * ) SI_UNIT ( .MILLI., .METRE. ) );
#3528 = FACE_BOUND ( 'NONE', #3819, .T. ) ;
#3529 = CARTESIAN_POINT ( 'NONE',  ( 199.9963296805737230, -4.796075449120964792E-12, -82.99999999999998579 ) ) ;
#3530 = ITEM_DEFINED_TRANSFORMATION ( 'NONE', 'NONE', #192,  #7485 ) ;
#3531 = CARTESIAN_POINT ( 'NONE',  ( 0.000000000000000000, 0.000000000000000000, -4.700000000000000178 ) ) ;
#3532 = PRODUCT_DEFINITION_CONTEXT ( 'detailed design', #2948, 'design' ) ;
#3533 = VERTEX_POINT ( 'NONE', #784 ) ;
#3534 = ORIENTED_EDGE ( 'NONE', *, *, #314, .F. ) ;
#3535 = CIRCLE ( 'NONE', #6310, 40.00000000000000000 ) ;
#3536 = CARTESIAN_POINT ( 'NONE',  ( 0.000000000000000000, 0.000000000000000000, 0.000000000000000000 ) ) ;
#3537 = CARTESIAN_POINT ( 'NONE',  ( 8.000000000000000000, 0.000000000000000000, 0.000000000000000000 ) ) ;
#3538 = FACE_OUTER_BOUND ( 'NONE', #5994, .T. ) ;
#3539 = DIRECTION ( 'NONE',  ( 0.3090169943749447867, 0.9510565162951546414, 0.000000000000000000 ) ) ;
#3540 = AXIS2_PLACEMENT_3D ( 'NONE', #6907, #6317, #900 ) ;
#3541 = CARTESIAN_POINT ( 'NONE',  ( 0.000000000000000000, 0.000000000000000000, -3.000000000000000000 ) ) ;
#3542 = DIRECTION ( 'NONE',  ( -0.000000000000000000, -0.000000000000000000, 1.000000000000000000 ) ) ;
#3543 = ORIENTED_EDGE ( 'NONE', *, *, #4867, .F. ) ;
#3544 = VERTEX_POINT ( 'NONE', #638 ) ;
#3545 = ORIENTED_EDGE ( 'NONE', *, *, #7068, .T. ) ;
#3546 = CARTESIAN_POINT ( 'NONE',  ( -3.500000000000007550, 3.710679801416480038E-15, 30.30000000000000071 ) ) ;
#3547 = CARTESIAN_POINT ( 'NONE',  ( -8.000000000000000000, -0.7805016046290998988, -3.388131789017200740E-17 ) ) ;
#3548 =( LENGTH_UNIT ( ) NAMED_UNIT ( * ) SI_UNIT ( .MILLI., .METRE. ) );
#3549 = ADVANCED_FACE ( 'NONE', ( #3714 ), #2578, .F. ) ;
#3550 = CARTESIAN_POINT ( 'NONE',  ( -68.76644452187068168, 49.96174644486002592, 24.17200000000001125 ) ) ;
#3551 = VERTEX_POINT ( 'NONE', #6082 ) ;
#3552 = VERTEX_POINT ( 'NONE', #3756 ) ;
#3553 = EDGE_CURVE ( 'NONE', #7551, #1947, #2908, .T. ) ;
#3554 = VECTOR ( 'NONE', #7159, 1000.000000000000000 ) ;
#3555 = CARTESIAN_POINT ( 'NONE',  ( 0.000000000000000000, 0.000000000000000000, 10.00000000000000000 ) ) ;
#3556 = DIRECTION ( 'NONE',  ( 0.000000000000000000, 0.000000000000000000, 1.000000000000000000 ) ) ;
#3557 = CARTESIAN_POINT ( 'NONE',  ( 0.000000000000000000, 0.000000000000000000, -139.9999999999999716 ) ) ;
#3558 = DIRECTION ( 'NONE',  ( 0.000000000000000000, -1.000000000000000000, 0.000000000000000000 ) ) ;
#3559 = CIRCLE ( 'NONE', #6840, 40.00000000000000711 ) ;
#3560 = EDGE_LOOP ( 'NONE', ( #5361, #7522, #5267, #7410 ) ) ;
#3561 = EDGE_CURVE ( 'NONE', #7346, #7759, #2709, .T. ) ;
#3562 = ORIENTED_EDGE ( 'NONE', *, *, #754, .F. ) ;
#3563 = EDGE_CURVE ( 'NONE', #3277, #886, #6054, .T. ) ;
#3564 = ORIENTED_EDGE ( 'NONE', *, *, #4947, .F. ) ;
#3565 = DIRECTION ( 'NONE',  ( -4.286207611454020849E-16, -1.000000000000000000, 0.000000000000000000 ) ) ;
#3566 = FACE_OUTER_BOUND ( 'NONE', #4446, .T. ) ;
#3567 = VECTOR ( 'NONE', #6734, 1000.000000000000000 ) ;
#3568 = ADVANCED_FACE ( 'NONE', ( #3636 ), #3661, .T. ) ;
#3569 = DIRECTION ( 'NONE',  ( 1.586032892321652729E-16, 1.000000000000000000, -0.000000000000000000 ) ) ;
#3570 = CARTESIAN_POINT ( 'NONE',  ( 119.9981648402868899, 207.8429183184021269, 10.00000000000000178 ) ) ;
#3571 = EDGE_CURVE ( 'NONE', #887, #6843, #6634, .T. ) ;
#3572 = LINE ( 'NONE', #6058, #2473 ) ;
#3573 = ORIENTED_EDGE ( 'NONE', *, *, #5287, .T. ) ;
#3574 = ORIENTED_EDGE ( 'NONE', *, *, #6844, .T. ) ;
#3575 = AXIS2_PLACEMENT_3D ( 'NONE', #778, #7374, #1821 ) ;
#3576 = CARTESIAN_POINT ( 'NONE',  ( -8.000000000000000000, 4.618802153517013842, -3.985468820183668104 ) ) ;
#3577 = DIRECTION ( 'NONE',  ( -1.000000000000000000, 0.000000000000000000, -0.000000000000000000 ) ) ;
#3578 = DIRECTION ( 'NONE',  ( -1.000000000000000000, 0.000000000000000000, 0.000000000000000000 ) ) ;
#3579 = DIRECTION ( 'NONE',  ( 0.000000000000000000, 0.000000000000000000, -1.000000000000000000 ) ) ;
#3580 = CIRCLE ( 'NONE', #173, 199.9963296805737230 ) ;
#3581 = FACE_OUTER_BOUND ( 'NONE', #1892, .T. ) ;
#3582 = ORIENTED_EDGE ( 'NONE', *, *, #946, .F. ) ;
#3583 = ORIENTED_EDGE ( 'NONE', *, *, #128, .T. ) ;
#3584 = VECTOR ( 'NONE', #3972, 1000.000000000000000 ) ;
#3585 = MECHANICAL_DESIGN_GEOMETRIC_PRESENTATION_REPRESENTATION (  '', ( #6481 ), #1829 ) ;
#3586 = ORIENTED_EDGE ( 'NONE', *, *, #7544, .F. ) ;
#3587 = CARTESIAN_POINT ( 'NONE',  ( 2.750000000000000000, -33.63777638310832430, 0.000000000000000000 ) ) ;
#3588 = FACE_OUTER_BOUND ( 'NONE', #2391, .T. ) ;
#3589 = LINE ( 'NONE', #592, #5207 ) ;
#3590 = PRODUCT_DEFINITION ( 'UNKNOWN', '', #38, #3532 ) ;
#3591 = AXIS2_PLACEMENT_3D ( 'NONE', #5626, #3260, #2670 ) ;
#3592 = COLOUR_RGB ( '',1.000000000000000000, 0.9490196078431372140, 0.9098039215686274384 ) ;
#3593 = PRODUCT_DEFINITION_SHAPE ( 'NONE', 'NONE',  #3590 ) ;
#3594 = ORIENTED_EDGE ( 'NONE', *, *, #3713, .F. ) ;
#3595 = VERTEX_POINT ( 'NONE', #1378 ) ;
#3596 = AXIS2_PLACEMENT_3D ( 'NONE', #2954, #6577, #5467 ) ;
#3597 = DIRECTION ( 'NONE',  ( 0.000000000000000000, 0.000000000000000000, -1.000000000000000000 ) ) ;
#3598 =( REPRESENTATION_RELATIONSHIP ('NONE','NONE', #1229, #1433 ) REPRESENTATION_RELATIONSHIP_WITH_TRANSFORMATION ( #572 )SHAPE_REPRESENTATION_RELATIONSHIP( ) );
#3599 = ADVANCED_FACE ( 'NONE', ( #1224 ), #711, .T. ) ;
#3600 = DIRECTION ( 'NONE',  ( -0.000000000000000000, -0.000000000000000000, 1.000000000000000000 ) ) ;
#3601 = CYLINDRICAL_SURFACE ( 'NONE', #5573, 10.00000000000000178 ) ;
#3602 = ADVANCED_FACE ( 'NONE', ( #2502 ), #4377, .T. ) ;
#3603 = EDGE_LOOP ( 'NONE', ( #272, #80, #904, #735 ) ) ;
#3604 = ADVANCED_FACE ( 'NONE', ( #3166 ), #5522, .F. ) ;
#3605 = ORIENTED_EDGE ( 'NONE', *, *, #6346, .F. ) ;
#3606 = ADVANCED_FACE ( 'NONE', ( #4890 ), #4970, .F. ) ;
#3607 = ORIENTED_EDGE ( 'NONE', *, *, #3173, .T. ) ;
#3608 = AXIS2_PLACEMENT_3D ( 'NONE', #1241, #5464, #6921 ) ;
#3609 = CYLINDRICAL_SURFACE ( 'NONE', #4359, 5.249999999999976907 ) ;
#3610 = CARTESIAN_POINT ( 'NONE',  ( 0.000000000000000000, 0.000000000000000000, -4.674599999999997202 ) ) ;
#3611 = DIRECTION ( 'NONE',  ( -0.000000000000000000, -0.000000000000000000, 1.000000000000000000 ) ) ;
#3612 = DIRECTION ( 'NONE',  ( 0.000000000000000000, 0.000000000000000000, 1.000000000000000000 ) ) ;
#3613 = ADVANCED_FACE ( 'NONE', ( #3086 ), #83, .F. ) ;
#3614 = PLANE ( 'NONE',  #1834 ) ;
#3615 = VERTEX_POINT ( 'NONE', #3127 ) ;
#3616 = CIRCLE ( 'NONE', #3484, 40.00000000000000711 ) ;
#3617 = B_SPLINE_CURVE_WITH_KNOTS ( 'NONE', 3,
 ( #3840, #1506, #241, #5054, #3914, #2151 ),
 .UNSPECIFIED., .F., .F.,
 ( 4, 2, 4 ),
 ( 2.380731629812508987E-07, 0.002336973833157575484, 0.004673709593152171327 ),
 .UNSPECIFIED. ) ;
#3618 = LINE ( 'NONE', #7281, #5174 ) ;
#3619 = CIRCLE ( 'NONE', #207, 29.99999999999999289 ) ;
#3620 = CARTESIAN_POINT ( 'NONE',  ( 26.82422866010496776, 9.628642520646589986, -122.9999999999999716 ) ) ;
#3621 = DIRECTION ( 'NONE',  ( 0.000000000000000000, 0.000000000000000000, -1.000000000000000000 ) ) ;
#3622 = DIRECTION ( 'NONE',  ( 0.9427735142430633264, -0.3334338027881765809, 1.931932416011734352E-18 ) ) ;
#3623 = CARTESIAN_POINT ( 'NONE',  ( -1.852913429038039572, -299.9999999999999432, -1041.954445729288636 ) ) ;
#3624 = CARTESIAN_POINT ( 'NONE',  ( -150.0000000000000568, 0.000000000000000000, 10.00000000000000000 ) ) ;
#3625 = DIRECTION ( 'NONE',  ( -0.000000000000000000, -0.000000000000000000, 1.000000000000000000 ) ) ;
#3626 = ORIENTED_EDGE ( 'NONE', *, *, #5334, .F. ) ;
#3627 = VECTOR ( 'NONE', #1206, 1000.000000000000000 ) ;
#3628 = ORIENTED_EDGE ( 'NONE', *, *, #1835, .F. ) ;
#3629 = ORIENTED_EDGE ( 'NONE', *, *, #558, .T. ) ;
#3630 = DIRECTION ( 'NONE',  ( 0.000000000000000000, 0.000000000000000000, -1.000000000000000000 ) ) ;
#3631 = AXIS2_PLACEMENT_3D ( 'NONE', #7582, #2197, #1398 ) ;
#3632 = DIRECTION ( 'NONE',  ( 1.000000000000000000, 0.000000000000000000, 0.000000000000000000 ) ) ;
#3633 = ORIENTED_EDGE ( 'NONE', *, *, #1826, .F. ) ;
#3634 = VERTEX_POINT ( 'NONE', #2540 ) ;
#3635 = CONICAL_SURFACE ( 'NONE', #7154, 4.999999999999990230, 0.7853981633974524978 ) ;
#3636 = FACE_OUTER_BOUND ( 'NONE', #4117, .T. ) ;
#3637 = CIRCLE ( 'NONE', #6793, 32.81578194438969120 ) ;
#3638 = CARTESIAN_POINT ( 'NONE',  ( -0.5700000000000001732, -28.49429942988597020, -3.000000000000000000 ) ) ;
#3639 = CARTESIAN_POINT ( 'NONE',  ( 3.499999999999996003, 4.574055794815363937E-15, 37.19999999999999574 ) ) ;
#3640 = ORIENTED_EDGE ( 'NONE', *, *, #3895, .T. ) ;
#3641 = AXIS2_PLACEMENT_3D ( 'NONE', #2240, #2902, #367 ) ;
#3642 = VERTEX_POINT ( 'NONE', #7342 ) ;
#3643 = DIRECTION ( 'NONE',  ( -0.000000000000000000, -0.000000000000000000, -1.000000000000000000 ) ) ;
#3644 = DIRECTION ( 'NONE',  ( 0.000000000000000000, 0.000000000000000000, 1.000000000000000000 ) ) ;
#3645 = DIRECTION ( 'NONE',  ( -1.000000000000000000, 0.000000000000000000, -0.000000000000000000 ) ) ;
#3646 = DIRECTION ( 'NONE',  ( 1.000000000000000000, 0.000000000000000000, 0.000000000000000000 ) ) ;
#3647 = ITEM_DEFINED_TRANSFORMATION ( 'NONE', 'NONE', #2225,  #7485 ) ;
#3648 = CIRCLE ( 'NONE', #2152, 5.249999999999997335 ) ;
#3649 = EDGE_CURVE ( 'NONE', #1854, #1053, #2779, .T. ) ;
#3650 = DIRECTION ( 'NONE',  ( -0.000000000000000000, -0.000000000000000000, -1.000000000000000000 ) ) ;
#3651 = ORIENTED_EDGE ( 'NONE', *, *, #3207, .T. ) ;
#3652 = CARTESIAN_POINT ( 'NONE',  ( -35.00000000000000711, 0.000000000000000000, -60.00000000000000711 ) ) ;
#3653 = EDGE_CURVE ( 'NONE', #7033, #6563, #7313, .T. ) ;
#3654 = FACE_BOUND ( 'NONE', #7069, .T. ) ;
#3655 = CYLINDRICAL_SURFACE ( 'NONE', #1222, 5.249999999999976907 ) ;
#3656 = DIRECTION ( 'NONE',  ( 1.849298671161525021E-17, 4.649428319898508021E-17, -0.9999999999999998890 ) ) ;
#3657 = PRODUCT_DEFINITION_SHAPE ( 'NONE', 'NONE',  #1223 ) ;
#3658 = PRESENTATION_STYLE_ASSIGNMENT (( #4951 ) ) ;
#3659 = DIRECTION ( 'NONE',  ( 0.000000000000000000, 0.000000000000000000, -1.000000000000000000 ) ) ;
#3661 = TOROIDAL_SURFACE ( 'NONE', #379, 37.19999999999999574, 0.3000000000000007661 ) ;
#3660 = CARTESIAN_POINT ( 'NONE',  ( -68.76644452187068168, 49.96174644486002592, -64.17200000000001125 ) ) ;
#3662 = VERTEX_POINT ( 'NONE', #5414 ) ;
#3663 = ORIENTED_EDGE ( 'NONE', *, *, #7331, .F. ) ;
#3664 = VERTEX_POINT ( 'NONE', #3979 ) ;
#3665 = AXIS2_PLACEMENT_3D ( 'NONE', #425, #384, #5795 ) ;
#3666 = LINE ( 'NONE', #74, #1519 ) ;
#3667 =( NAMED_UNIT ( * ) SI_UNIT ( $, .STERADIAN. ) SOLID_ANGLE_UNIT ( ) );
#3668 = APPLICATION_PROTOCOL_DEFINITION ( 'draft international standard', 'automotive_design', 1998, #6621 ) ;
#3669 = DIRECTION ( 'NONE',  ( -0.000000000000000000, -0.000000000000000000, 1.000000000000000000 ) ) ;
#3670 = EDGE_CURVE ( 'NONE', #5491, #887, #6936, .T. ) ;
#3671 = VERTEX_POINT ( 'NONE', #2723 ) ;
#3672 = CIRCLE ( 'NONE', #5049, 35.97500000000000853 ) ;
#3673 = ORIENTED_EDGE ( 'NONE', *, *, #3793, .F. ) ;
#3674 = DIRECTION ( 'NONE',  ( 1.000000000000000000, 0.000000000000000000, 0.000000000000000000 ) ) ;
#3675 = CARTESIAN_POINT ( 'NONE',  ( -4.000000000000004441, -6.928203230275506108, 0.000000000000000000 ) ) ;
#3676 = DIRECTION ( 'NONE',  ( 3.081487911019577365E-33, -2.775557561562891967E-17, -1.000000000000000000 ) ) ;
#3677 = VERTEX_POINT ( 'NONE', #5603 ) ;
#3678 = ORIENTED_EDGE ( 'NONE', *, *, #795, .T. ) ;
#3679 = FACE_OUTER_BOUND ( 'NONE', #1173, .T. ) ;
#3680 = DIRECTION ( 'NONE',  ( -0.000000000000000000, -0.000000000000000000, -1.000000000000000000 ) ) ;
#3681 = CARTESIAN_POINT ( 'NONE',  ( -213.0929183184020701, 119.9981648402869467, 10.00000000000000000 ) ) ;
#3682 = DIRECTION ( 'NONE',  ( -1.000000000000000000, 0.000000000000000000, 0.000000000000000000 ) ) ;
#3683 = CONTEXT_DEPENDENT_SHAPE_REPRESENTATION ( #6021, #65 ) ;
#3684 = DIRECTION ( 'NONE',  ( 1.000000000000000000, 0.000000000000000000, 0.000000000000000000 ) ) ;
#3685 = ADVANCED_FACE ( 'NONE', ( #2142 ), #6390, .T. ) ;
#3686 = ORIENTED_EDGE ( 'NONE', *, *, #4179, .T. ) ;
#3687 = AXIS2_PLACEMENT_3D ( 'NONE', #3474, #4536, #1539 ) ;
#3688 = AXIS2_PLACEMENT_3D ( 'NONE', #2952, #3498, #454 ) ;
#3689 = DIRECTION ( 'NONE',  ( 0.000000000000000000, 0.000000000000000000, 1.000000000000000000 ) ) ;
#3690 = FACE_OUTER_BOUND ( 'NONE', #6405, .T. ) ;
#3691 = PLANE ( 'NONE',  #6271 ) ;
#3692 = DIRECTION ( 'NONE',  ( 0.9845265360683709277, 0.1752355551171481118, -5.551115123125782702E-17 ) ) ;
#3693 = DIRECTION ( 'NONE',  ( -0.000000000000000000, 1.000000000000000000, 1.224646799147353207E-16 ) ) ;
#3694 = EDGE_CURVE ( 'NONE', #6870, #3153, #12, .T. ) ;
#3695 = CARTESIAN_POINT ( 'NONE',  ( -20.63749999999999574, 0.000000000000000000, 0.000000000000000000 ) ) ;
#3696 = AXIS2_PLACEMENT_3D ( 'NONE', #6524, #7197, #5976 ) ;
#3697 = CARTESIAN_POINT ( 'NONE',  ( -3.199999999999996181, 0.000000000000000000, -37.19999999999999574 ) ) ;
#3698 = EDGE_CURVE ( 'NONE', #3533, #2245, #5927, .T. ) ;
#3699 = ORIENTED_EDGE ( 'NONE', *, *, #935, .F. ) ;
#3700 = EDGE_CURVE ( 'NONE', #1573, #5335, #1008, .T. ) ;
#3701 = VERTEX_POINT ( 'NONE', #939 ) ;
#3702 = EDGE_CURVE ( 'NONE', #6571, #7478, #6430, .T. ) ;
#3703 = ORIENTED_EDGE ( 'NONE', *, *, #1929, .F. ) ;
#3704 = AXIS2_PLACEMENT_3D ( 'NONE', #5743, #1279, #3689 ) ;
#3705 = AXIS2_PLACEMENT_3D ( 'NONE', #1368, #4332, #113 ) ;
#3706 = CARTESIAN_POINT ( 'NONE',  ( 8.000000000000000000, -4.618802153517011178, -0.7145311798163319628 ) ) ;
#3707 = DIRECTION ( 'NONE',  ( 0.000000000000000000, 0.000000000000000000, -1.000000000000000000 ) ) ;
#3708 = EDGE_CURVE ( 'NONE', #5120, #3378, #3038, .T. ) ;
#3709 = AXIS2_PLACEMENT_3D ( 'NONE', #1009, #1089, #4762 ) ;
#3710 = ORIENTED_EDGE ( 'NONE', *, *, #4403, .F. ) ;
#3711 = CIRCLE ( 'NONE', #2078, 29.99999999999999289 ) ;
#3712 = ORIENTED_EDGE ( 'NONE', *, *, #2553, .F. ) ;
#3713 = EDGE_CURVE ( 'NONE', #4996, #4712, #760, .T. ) ;
#3714 = FACE_OUTER_BOUND ( 'NONE', #4569, .T. ) ;
#3716 = AXIS2_PLACEMENT_3D ( 'NONE', #2905, #2199, #7042 ) ;
#3715 = CARTESIAN_POINT ( 'NONE',  ( -8.000000000000001776, -3.098204225878176121, -4.384209322808125364 ) ) ;
#3717 = DIRECTION ( 'NONE',  ( -0.7071067811865474617, 8.659560562354932858E-17, 0.7071067811865474617 ) ) ;
#3718 = FACE_OUTER_BOUND ( 'NONE', #4001, .T. ) ;
#3719 = ORIENTED_EDGE ( 'NONE', *, *, #3810, .F. ) ;
#3720 = ORIENTED_EDGE ( 'NONE', *, *, #3122, .T. ) ;
#3721 = PRODUCT ( 'base plate', 'base plate', '', ( #6142 ) ) ;
#3722 = DIRECTION ( 'NONE',  ( -0.000000000000000000, -0.000000000000000000, 1.000000000000000000 ) ) ;
#3723 = DIRECTION ( 'NONE',  ( 0.000000000000000000, 0.000000000000000000, -1.000000000000000000 ) ) ;
#3724 = DIRECTION ( 'NONE',  ( -0.000000000000000000, -0.000000000000000000, 1.000000000000000000 ) ) ;
#3725 = CARTESIAN_POINT ( 'NONE',  ( -4.586480920263581673, -37.21846574978686562, -3.000000000000000000 ) ) ;
#3726 = CARTESIAN_POINT ( 'NONE',  ( -1.677050983124841466, 0.000000000000000000, 0.000000000000000000 ) ) ;
#3727 = AXIS2_PLACEMENT_3D ( 'NONE', #4524, #7555, #2168 ) ;
#3728 = ORIENTED_EDGE ( 'NONE', *, *, #7657, .F. ) ;
#3729=STYLED_ITEM('',(#7830),#475);
#3730 = LINE ( 'NONE', #5428, #1143 ) ;
#3731 = CARTESIAN_POINT ( 'NONE',  ( 10.16320117273318679, -26.62629042736811869, -122.9999999999999716 ) ) ;
#3732 = CARTESIAN_POINT ( 'NONE',  ( -5.249999999999972466, 239.9963296805737230, 10.00000000000000178 ) ) ;
#3733 = DIRECTION ( 'NONE',  ( -0.8900306386520617785, 0.4559007153543442326, -2.550145071705742900E-17 ) ) ;
#3734 = CIRCLE ( 'NONE', #1465, 29.99999999999999289 ) ;
#3735 = CARTESIAN_POINT ( 'NONE',  ( 3.716043017018883621, 28.25669875083898930, 13.00000000000000178 ) ) ;
#3736 = CARTESIAN_POINT ( 'NONE',  ( -6.713333333332999864, 9.009318285727158319E-16, 3.859999999999999876 ) ) ;
#3737 = LINE ( 'NONE', #6032, #3070 ) ;
#3738 = VERTEX_POINT ( 'NONE', #7452 ) ;
#3739 = ORIENTED_EDGE ( 'NONE', *, *, #5436, .T. ) ;
#3740 = CIRCLE ( 'NONE', #7390, 5.249999999999995559 ) ;
#3741 = EDGE_CURVE ( 'NONE', #380, #5243, #4455, .T. ) ;
#3742 = ORIENTED_EDGE ( 'NONE', *, *, #6939, .F. ) ;
#3743 = CARTESIAN_POINT ( 'NONE',  ( 0.000000000000000000, 0.000000000000000000, -4.700000000000000178 ) ) ;
#3744 = CARTESIAN_POINT ( 'NONE',  ( 8.000000000000000000, -4.618802153517011178, -3.985468820183668104 ) ) ;
#3745 = EDGE_CURVE ( 'NONE', #599, #6897, #2284, .T. ) ;
#3746 = PRESENTATION_STYLE_ASSIGNMENT (( #3046 ) ) ;
#3747 = EDGE_CURVE ( 'NONE', #2556, #6929, #6236, .T. ) ;
#3748 = CARTESIAN_POINT ( 'NONE',  ( -68.76644452187072432, 49.96174644486006855, -134.1720000000000255 ) ) ;
#3749 = AXIS2_PLACEMENT_3D ( 'NONE', #958, #3375, #3334 ) ;
#3750 = EDGE_CURVE ( 'NONE', #1170, #3677, #6186, .T. ) ;
#3751 = ORIENTED_EDGE ( 'NONE', *, *, #3561, .T. ) ;
#3752 = ORIENTED_EDGE ( 'NONE', *, *, #6300, .T. ) ;
#3753 =( REPRESENTATION_RELATIONSHIP ('NONE','NONE', #1229, #1433 ) REPRESENTATION_RELATIONSHIP_WITH_TRANSFORMATION ( #5021 )SHAPE_REPRESENTATION_RELATIONSHIP( ) );
#3754 = ORIENTED_EDGE ( 'NONE', *, *, #3134, .T. ) ;
#3755 = CIRCLE ( 'NONE', #1103, 30.00000000000000000 ) ;
#3756 = CARTESIAN_POINT ( 'NONE',  ( -5.249999999999962697, 239.9963296805737230, -8.673617379884035472E-15 ) ) ;
#3757 = EDGE_CURVE ( 'NONE', #5317, #3377, #6688, .T. ) ;
#3758 = DIRECTION ( 'NONE',  ( 0.000000000000000000, 0.000000000000000000, 1.000000000000000000 ) ) ;
#3759 = CARTESIAN_POINT ( 'NONE',  ( -58.76644452187068168, 49.96174644486002592, -40.00000000000000000 ) ) ;
#3760 = CARTESIAN_POINT ( 'NONE',  ( -30.00000000000000000, 3.673940397442059178E-15, 0.000000000000000000 ) ) ;
#3761 = EDGE_LOOP ( 'NONE', ( #1393, #7371, #3300, #973 ) ) ;
#3762 = AXIS2_PLACEMENT_3D ( 'NONE', #4466, #7535, #3365 ) ;
#3763 = ORIENTED_EDGE ( 'NONE', *, *, #5185, .T. ) ;
#3764 = DIRECTION ( 'NONE',  ( -1.000000000000000000, 8.881784197001252323E-16, 0.000000000000000000 ) ) ;
#3765 = DIRECTION ( 'NONE',  ( -0.09063257223759993431, -0.9958843993404034034, 0.000000000000000000 ) ) ;
#3766 = AXIS2_PLACEMENT_3D ( 'NONE', #235, #3795, #5013 ) ;
#3767 = DIRECTION ( 'NONE',  ( -0.000000000000000000, -0.000000000000000000, 1.000000000000000000 ) ) ;
#3768 = CARTESIAN_POINT ( 'NONE',  ( -114.7481648402875578, 207.8429183184017859, -120.0000000000000000 ) ) ;
#3769 = ORIENTED_EDGE ( 'NONE', *, *, #2012, .F. ) ;
#3770 = CYLINDRICAL_SURFACE ( 'NONE', #5119, 5.249999999999976907 ) ;
#3771 = CARTESIAN_POINT ( 'NONE',  ( 2.583028308771596837, 28.38270538120150377, 13.00000000000000178 ) ) ;
#3772 = AXIS2_PLACEMENT_3D ( 'NONE', #5936, #1911, #3058 ) ;
#3773 = CARTESIAN_POINT ( 'NONE',  ( 0.000000000000000000, 0.000000000000000000, -50.00000000000000000 ) ) ;
#3774 = CARTESIAN_POINT ( 'NONE',  ( 29.99999999999999289, 0.000000000000000000, -139.9999999999999716 ) ) ;
#3775 = PRODUCT_CONTEXT ( 'NONE', #7169, 'mechanical' ) ;
#3776 = SURFACE_STYLE_USAGE ( .BOTH. , #2600 ) ;
#3777 = DIRECTION ( 'NONE',  ( -0.7071067811865504593, 0.000000000000000000, -0.7071067811865445751 ) ) ;
#3778 = EDGE_LOOP ( 'NONE', ( #2526, #3042, #307, #1019 ) ) ;
#3779 = AXIS2_PLACEMENT_3D ( 'NONE', #1649, #3542, #6457 ) ;
#3780 = ORIENTED_EDGE ( 'NONE', *, *, #3026, .F. ) ;
#3781 = ORIENTED_EDGE ( 'NONE', *, *, #1276, .T. ) ;
#3782 = CARTESIAN_POINT ( 'NONE',  ( -10.00000000000000000, 33.54101966249685773, -50.00000000000000000 ) ) ;
#3783 =( NAMED_UNIT ( * ) SI_UNIT ( $, .STERADIAN. ) SOLID_ANGLE_UNIT ( ) );
#3784 = COLOUR_RGB ( '',0.8941176470588234615, 0.8941176470588234615, 0.8941176470588234615 ) ;
#3785 = CARTESIAN_POINT ( 'NONE',  ( -11.50644898236017433, -35.69105814929478981, -3.000000000000000000 ) ) ;
#3786 = PRODUCT_DEFINITION ( 'UNKNOWN', '', #1674, #6700 ) ;
#3787 = VERTEX_POINT ( 'NONE', #3868 ) ;
#3788 = PRODUCT ( 'MAS-196', 'MAS-196', '', ( #7605 ) ) ;
#3789 = ORIENTED_EDGE ( 'NONE', *, *, #573, .F. ) ;
#3790 = EDGE_LOOP ( 'NONE', ( #1316, #5982, #42, #2762 ) ) ;
#3791 = AXIS2_PLACEMENT_3D ( 'NONE', #1185, #5253, #5329 ) ;
#3792 = ADVANCED_FACE ( 'NONE', ( #5755 ), #1647, .T. ) ;
#3793 = EDGE_CURVE ( 'NONE', #3132, #1496, #2178, .T. ) ;
#3794 = CARTESIAN_POINT ( 'NONE',  ( 119.9981648402868899, 207.8429183184021269, 10.00000000000000000 ) ) ;
#3795 = DIRECTION ( 'NONE',  ( 1.000000000000000000, 0.000000000000000000, 0.000000000000000000 ) ) ;
#3796 = CIRCLE ( 'NONE', #765, 8.000000000000000000 ) ;
#3797 = CARTESIAN_POINT ( 'NONE',  ( -26.82422866010495710, -9.628642520646591763, -119.9999999999999716 ) ) ;
#3798 = ORIENTED_EDGE ( 'NONE', *, *, #5640, .F. ) ;
#3799 = AXIS2_PLACEMENT_3D ( 'NONE', #2367, #4757, #5309 ) ;
#3800 = ADVANCED_FACE ( 'NONE', ( #3279 ), #6983, .T. ) ;
#3801 = ADVANCED_FACE ( 'NONE', ( #4494 ), #1265, .T. ) ;
#3802 = CARTESIAN_POINT ( 'NONE',  ( -3.319543390096037605, 7.321065037175422674, -0.01688885742776584376 ) ) ;
#3803 = CARTESIAN_POINT ( 'NONE',  ( -114.7481648402868188, 207.8429183184021554, -8.673617379884035472E-15 ) ) ;
#3804 = CARTESIAN_POINT ( 'NONE',  ( 29.99999999999999289, 0.000000000000000000, -50.00000000000000000 ) ) ;
#3805 = DIRECTION ( 'NONE',  ( -0.000000000000000000, -0.000000000000000000, 1.000000000000000000 ) ) ;
#3806 = ORIENTED_EDGE ( 'NONE', *, *, #4529, .F. ) ;
#3807 = ADVANCED_FACE ( 'NONE', ( #3315 ), #4612, .F. ) ;
#3808 = DIRECTION ( 'NONE',  ( 1.000000000000000000, 0.000000000000000000, 0.000000000000000000 ) ) ;
#3809 = CYLINDRICAL_SURFACE ( 'NONE', #4985, 10.00000000000000178 ) ;
#3810 = EDGE_CURVE ( 'NONE', #3939, #5401, #2341, .T. ) ;
#3811 = VECTOR ( 'NONE', #6248, 1000.000000000000000 ) ;
#3812 = DIRECTION ( 'NONE',  ( -0.000000000000000000, -0.000000000000000000, -1.000000000000000000 ) ) ;
#3813 = CARTESIAN_POINT ( 'NONE',  ( 8.000000000000000000, 0.000000000000000000, -4.700000000000000178 ) ) ;
#3814 = APPLICATION_PROTOCOL_DEFINITION ( 'draft international standard', 'automotive_design', 1998, #1624 ) ;
#3815 = LINE ( 'NONE', #4439, #4971 ) ;
#3816 = DIRECTION ( 'NONE',  ( 0.000000000000000000, 0.000000000000000000, 1.000000000000000000 ) ) ;
#3817 = ORIENTED_EDGE ( 'NONE', *, *, #1380, .T. ) ;
#3818 = ORIENTED_EDGE ( 'NONE', *, *, #4655, .F. ) ;
#3819 = EDGE_LOOP ( 'NONE', ( #4753, #1070 ) ) ;
#3820 = ORIENTED_EDGE ( 'NONE', *, *, #5128, .F. ) ;
#3821 = ORIENTED_EDGE ( 'NONE', *, *, #508, .T. ) ;
#3822 = DIRECTION ( 'NONE',  ( -1.000000000000000000, 8.881784197001252323E-16, 0.000000000000000000 ) ) ;
#3823 = FILL_AREA_STYLE_COLOUR ( '', #3784 ) ;
#3824 = AXIS2_PLACEMENT_3D ( 'NONE', #3177, #91, #4903 ) ;
#3825 = CARTESIAN_POINT ( 'NONE',  ( -10.00000000000000000, 28.28427124746190202, 0.000000000000000000 ) ) ;
#3826 = EDGE_LOOP ( 'NONE', ( #5228, #1014 ) ) ;
#3827 = VERTEX_POINT ( 'NONE', #5835 ) ;
#3828 = AXIS2_PLACEMENT_3D ( 'NONE', #3550, #7724, #5836 ) ;
#3829 = DIRECTION ( 'NONE',  ( 1.000000000000000000, 0.000000000000000000, 0.000000000000000000 ) ) ;
#3830 = SURFACE_STYLE_FILL_AREA ( #2026 ) ;
#3831 = CARTESIAN_POINT ( 'NONE',  ( -74.01644452187068168, 49.96174644486002592, 10.00000000000000000 ) ) ;
#3832=STYLED_ITEM('',(#7830),#5676);
#3833 = CIRCLE ( 'NONE', #2960, 37.19999999999999574 ) ;
#3834 = DIRECTION ( 'NONE',  ( 1.000000000000000000, 0.000000000000000000, 0.000000000000000000 ) ) ;
#3835 = ORIENTED_EDGE ( 'NONE', *, *, #362, .T. ) ;
#3836=STYLED_ITEM('',(#7830),#5741);
#3837 = EDGE_CURVE ( 'NONE', #4532, #3942, #2379, .T. ) ;
#3838 = PLANE ( 'NONE',  #2856 ) ;
#3839 = LINE ( 'NONE', #6914, #5974 ) ;
#3840 = CARTESIAN_POINT ( 'NONE',  ( -2.081668171172168513E-14, -9.237604307034017026, -3.985468820183668104 ) ) ;
#3841 = EDGE_CURVE ( 'NONE', #1983, #6200, #4984, .T. ) ;
#3842 = EDGE_CURVE ( 'NONE', #7033, #7338, #2290, .T. ) ;
#3843 = LINE ( 'NONE', #3880, #2180 ) ;
#3844 = CIRCLE ( 'NONE', #6238, 29.99999999999999289 ) ;
#3845 = ORIENTED_EDGE ( 'NONE', *, *, #4042, .F. ) ;
#3846 = MECHANICAL_DESIGN_GEOMETRIC_PRESENTATION_REPRESENTATION (  '', ( #5856 ), #4725 ) ;
#3847 = ADVANCED_FACE ( 'NONE', ( #7178 ), #4051, .F. ) ;
#3848 = PLANE ( 'NONE',  #6896 ) ;
#3849 = CYLINDRICAL_SURFACE ( 'NONE', #3861, 37.49999999999997868 ) ;
#3850 = EDGE_CURVE ( 'NONE', #3551, #4484, #3796, .T. ) ;
#3851 = AXIS2_PLACEMENT_3D ( 'NONE', #5788, #4087, #1048 ) ;
#3852 = AXIS2_PLACEMENT_3D ( 'NONE', #5353, #7632, #5268 ) ;
#3853 = CARTESIAN_POINT ( 'NONE',  ( -68.76644452187068168, 49.96174644486002592, -40.00000000000000000 ) ) ;
#3854 = CARTESIAN_POINT ( 'NONE',  ( -199.9963296805737230, 0.000000000000000000, 10.00000000000000000 ) ) ;
#3855 = PRODUCT_DEFINITION_SHAPE ( 'NONE', 'NONE',  #7768 ) ;
#3856 = DIRECTION ( 'NONE',  ( 0.000000000000000000, 0.000000000000000000, 1.000000000000000000 ) ) ;
#3857 = VERTEX_POINT ( 'NONE', #3546 ) ;
#3858 = ORIENTED_EDGE ( 'NONE', *, *, #2017, .T. ) ;
#3859 = ORIENTED_EDGE ( 'NONE', *, *, #3362, .T. ) ;
#3860 = EDGE_LOOP ( 'NONE', ( #2315, #5636, #6119, #1227 ) ) ;
#3861 = AXIS2_PLACEMENT_3D ( 'NONE', #7431, #2080, #4510 ) ;
#3862 = CARTESIAN_POINT ( 'NONE',  ( -0.3344772040064616925, 0.000000000000000000, 0.000000000000000000 ) ) ;
#3863 = DIRECTION ( 'NONE',  ( -0.000000000000000000, -0.000000000000000000, 1.000000000000000000 ) ) ;
#3864 = CARTESIAN_POINT ( 'NONE',  ( -2.750000000000000000, -33.63777638310832430, 0.000000000000000000 ) ) ;
#3865 = ORIENTED_EDGE ( 'NONE', *, *, #3232, .T. ) ;
#3866 = AXIS2_PLACEMENT_3D ( 'NONE', #2930, #3434, #1622 ) ;
#3867 = EDGE_LOOP ( 'NONE', ( #701, #4554, #2141, #7439 ) ) ;
#3868 = CARTESIAN_POINT ( 'NONE',  ( 5.857142857142856762, 0.000000000000000000, 2.573333333332999739 ) ) ;
#3869 = AXIS2_PLACEMENT_3D ( 'NONE', #441, #4108, #3958 ) ;
#3870 = DIRECTION ( 'NONE',  ( 1.000000000000000000, 0.000000000000000000, 0.000000000000000000 ) ) ;
#3871 = LINE ( 'NONE', #6165, #6795 ) ;
#3872 = DIRECTION ( 'NONE',  ( 0.000000000000000000, 0.000000000000000000, -1.000000000000000000 ) ) ;
#3873 = VERTEX_POINT ( 'NONE', #1784 ) ;
#3874 = CIRCLE ( 'NONE', #6713, 28.50000000000000711 ) ;
#3875 = DIRECTION ( 'NONE',  ( -0.000000000000000000, -0.000000000000000000, -1.000000000000000000 ) ) ;
#3876 = CARTESIAN_POINT ( 'NONE',  ( 145.1064334105738567, -38.00161816110871627, 5.000000000000000000 ) ) ;
#3877 = CARTESIAN_POINT ( 'NONE',  ( 5.777789833161707559E-31, -4.119912841284263785E-15, -119.9999999999999716 ) ) ;
#3878 = ITEM_DEFINED_TRANSFORMATION ( 'NONE', 'NONE', #3938,  #7485 ) ;
#3879 = AXIS2_PLACEMENT_3D ( 'NONE', #4197, #6683, #6609 ) ;
#3880 = CARTESIAN_POINT ( 'NONE',  ( 145.1064334105730893, 38.00161816111175739, 5.000000000000000000 ) ) ;
#3881 = VERTEX_POINT ( 'NONE', #5279 ) ;
#3882 = CARTESIAN_POINT ( 'NONE',  ( 0.000000000000000000, 0.000000000000000000, 10.00000000000000000 ) ) ;
#3883 = VECTOR ( 'NONE', #2621, 1000.000000000000000 ) ;
#3884 = CARTESIAN_POINT ( 'NONE',  ( 9.702951051037011609, -29.86427928513813868, -3.000000000000000000 ) ) ;
#3885 = FACE_OUTER_BOUND ( 'NONE', #5707, .T. ) ;
#3886 = ADVANCED_FACE ( 'NONE', ( #2222 ), #3414, .T. ) ;
#3887 = CARTESIAN_POINT ( 'NONE',  ( 279.9963296805736945, -6.714540835673234486E-12, 576.0908266162076643 ) ) ;
#3888 = DIRECTION ( 'NONE',  ( -1.000000000000000000, 0.000000000000000000, 0.000000000000000000 ) ) ;
#3889 = SHAPE_DEFINITION_REPRESENTATION ( #3657, #5768 ) ;
#3890 = CIRCLE ( 'NONE', #3259, 5.857142857142855874 ) ;
#3891 = DIRECTION ( 'NONE',  ( 0.000000000000000000, 0.000000000000000000, 1.000000000000000000 ) ) ;
#3892 = ORIENTED_EDGE ( 'NONE', *, *, #7735, .F. ) ;
#3893 = EDGE_LOOP ( 'NONE', ( #1151, #7214, #6669, #1960 ) ) ;
#3894 = ORIENTED_EDGE ( 'NONE', *, *, #1780, .T. ) ;
#3895 = EDGE_CURVE ( 'NONE', #4594, #2925, #2803, .T. ) ;
#3896 = VECTOR ( 'NONE', #3611, 1000.000000000000000 ) ;
#3897 = ORIENTED_EDGE ( 'NONE', *, *, #4850, .T. ) ;
#3898 = DIRECTION ( 'NONE',  ( -0.000000000000000000, -0.000000000000000000, -1.000000000000000000 ) ) ;
#3899 = DIRECTION ( 'NONE',  ( 0.000000000000000000, 0.000000000000000000, 1.000000000000000000 ) ) ;
#3900 = CARTESIAN_POINT ( 'NONE',  ( 5.870234470492294880E-31, -4.203179568131150526E-15, -122.9999999999999716 ) ) ;
#3901 = CIRCLE ( 'NONE', #5281, 8.000000000000000000 ) ;
#3902 = ORIENTED_EDGE ( 'NONE', *, *, #3895, .F. ) ;
#3903 = VERTEX_POINT ( 'NONE', #3427 ) ;
#3904 = EDGE_LOOP ( 'NONE', ( #5820, #2285, #1726, #6451 ) ) ;
#3905 = AXIS2_PLACEMENT_3D ( 'NONE', #855, #3305, #6935 ) ;
#3906 = DIRECTION ( 'NONE',  ( -0.000000000000000000, -0.000000000000000000, 1.000000000000000000 ) ) ;
#3907 = EDGE_CURVE ( 'NONE', #5665, #1972, #6061, .T. ) ;
#3908 = PLANE ( 'NONE',  #4899 ) ;
#3909 = CARTESIAN_POINT ( 'NONE',  ( 0.000000000000000000, 0.000000000000000000, 2.573333333332999739 ) ) ;
#3910 = ORIENTED_EDGE ( 'NONE', *, *, #6636, .F. ) ;
#3911 = CARTESIAN_POINT ( 'NONE',  ( 213.0929183184020701, 119.9981648402868331, -8.673617379884035472E-15 ) ) ;
#3912 = CARTESIAN_POINT ( 'NONE',  ( -63.51644452187067458, 49.96174644486002592, 10.00000000000000000 ) ) ;
#3913 = CONICAL_SURFACE ( 'NONE', #6190, 8.000000000000000000, 1.047197551196596299 ) ;
#3914 = CARTESIAN_POINT ( 'NONE',  ( -3.318518101603016746, -7.321656987762879432, -4.700000000000000178 ) ) ;
#3915 = CARTESIAN_POINT ( 'NONE',  ( 10.69810649761387822, -28.02767413407169528, -119.9999999999999716 ) ) ;
#3916 = EDGE_LOOP ( 'NONE', ( #4402, #5080, #5549, #4519 ) ) ;
#3917 = FACE_BOUND ( 'NONE', #1533, .T. ) ;
#3918 = DIRECTION ( 'NONE',  ( 1.000000000000000000, 0.000000000000000000, 0.000000000000000000 ) ) ;
#3919 = CARTESIAN_POINT ( 'NONE',  ( 10.00000000000000000, 28.28427124746189136, -50.00000000000000000 ) ) ;
#3920 = EDGE_CURVE ( 'NONE', #952, #387, #7138, .T. ) ;
#3921 = CARTESIAN_POINT ( 'NONE',  ( 5.857142857142855874, 0.000000000000000000, 3.859999999999999876 ) ) ;
#3922 = FACE_BOUND ( 'NONE', #577, .T. ) ;
#3923 = CARTESIAN_POINT ( 'NONE',  ( -64.59444452187068464, 49.96174644486002592, 25.00000000000000000 ) ) ;
#3924 = ORIENTED_EDGE ( 'NONE', *, *, #6407, .F. ) ;
#3925 = ORIENTED_EDGE ( 'NONE', *, *, #7644, .T. ) ;
#3926 = EDGE_LOOP ( 'NONE', ( #2528, #5199, #222, #482 ) ) ;
#3927 = EDGE_CURVE ( 'NONE', #6002, #7492, #2788, .T. ) ;
#3928 = CIRCLE ( 'NONE', #3060, 37.50000000000000000 ) ;
#3929 = ORIENTED_EDGE ( 'NONE', *, *, #4120, .F. ) ;
#3930 = EDGE_CURVE ( 'NONE', #7135, #293, #6941, .T. ) ;
#3931 = CARTESIAN_POINT ( 'NONE',  ( -68.76644452187068168, 49.96174644486002592, 25.00000000000000000 ) ) ;
#3932 = DIRECTION ( 'NONE',  ( 0.000000000000000000, 1.000000000000000000, 0.000000000000000000 ) ) ;
#3933 = DIRECTION ( 'NONE',  ( 0.3090169943749582204, -0.9510565162951500895, 0.000000000000000000 ) ) ;
#3934 = LINE ( 'NONE', #3236, #1429 ) ;
#3935 = ADVANCED_FACE ( 'NONE', ( #6507 ), #7097, .T. ) ;
#3936 = AXIS2_PLACEMENT_3D ( 'NONE', #6326, #6842, #7388 ) ;
#3937 = EDGE_CURVE ( 'NONE', #545, #4638, #505, .T. ) ;
#3938 = AXIS2_PLACEMENT_3D ( 'NONE', #3107, #102, #2523 ) ;
#3939 = VERTEX_POINT ( 'NONE', #2962 ) ;
#3940 = EDGE_CURVE ( 'NONE', #6520, #491, #5318, .T. ) ;
#3941 = ORIENTED_EDGE ( 'NONE', *, *, #1377, .F. ) ;
#3942 = VERTEX_POINT ( 'NONE', #5514 ) ;
#3943 = AXIS2_PLACEMENT_3D ( 'NONE', #4689, #2262, #1581 ) ;
#3944 = DIRECTION ( 'NONE',  ( 1.000000000000000000, 0.000000000000000000, 0.000000000000000000 ) ) ;
#3945 = ADVANCED_FACE ( 'NONE', ( #6628 ), #3913, .T. ) ;
#3946 = CARTESIAN_POINT ( 'NONE',  ( -119.9981648402875578, 207.8429183184017859, -50.00000000000000000 ) ) ;
#3947 = DIRECTION ( 'NONE',  ( 1.000000000000000000, 0.000000000000000000, 0.000000000000000000 ) ) ;
#3948 = CIRCLE ( 'NONE', #6091, 37.49999999999997868 ) ;
#3949 = ORIENTED_EDGE ( 'NONE', *, *, #5238, .F. ) ;
#3950 = ADVANCED_FACE ( 'NONE', ( #110 ), #2530, .T. ) ;
#3951 = PLANE ( 'NONE',  #1336 ) ;
#3952 = DIRECTION ( 'NONE',  ( 1.000000000000000000, 0.000000000000000000, 0.000000000000000000 ) ) ;
#3953 = CARTESIAN_POINT ( 'NONE',  ( 5.238334947888644955, -36.57199107895616663, -3.000000000000000000 ) ) ;
#3954 = DIRECTION ( 'NONE',  ( 1.000000000000000000, 0.000000000000000000, 0.000000000000000000 ) ) ;
#3955 = VERTEX_POINT ( 'NONE', #3706 ) ;
#3956 = PRESENTATION_LAYER_ASSIGNMENT (  '', '', ( #1054 ) ) ;
#3957 = AXIS2_PLACEMENT_3D ( 'NONE', #5803, #3322, #6875 ) ;
#3958 = DIRECTION ( 'NONE',  ( -1.000000000000000000, 0.000000000000000000, 0.000000000000000000 ) ) ;
#3959 = CARTESIAN_POINT ( 'NONE',  ( 0.7499999999999730216, -37.49249924984995630, -3.000000000000000000 ) ) ;
#3960 = CARTESIAN_POINT ( 'NONE',  ( -0.7500000000000000000, -37.49249924984995630, -3.000000000000000000 ) ) ;
#3961 = DIRECTION ( 'NONE',  ( -0.000000000000000000, -0.000000000000000000, 1.000000000000000000 ) ) ;
#3962 = DIRECTION ( 'NONE',  ( 0.000000000000000000, 0.000000000000000000, -1.000000000000000000 ) ) ;
#3963 = PRESENTATION_LAYER_ASSIGNMENT (  '', '', ( #6481 ) ) ;
#3964 = CARTESIAN_POINT ( 'NONE',  ( 0.000000000000000000, 0.000000000000000000, -139.9999999999999716 ) ) ;
#3965 = ORIENTED_EDGE ( 'NONE', *, *, #3694, .F. ) ;
#3966 = ORIENTED_EDGE ( 'NONE', *, *, #562, .T. ) ;
#3967 = EDGE_LOOP ( 'NONE', ( #5256, #4298, #6212, #1758 ) ) ;
#3968 = ORIENTED_EDGE ( 'NONE', *, *, #4183, .T. ) ;
#3969 = LINE ( 'NONE', #1563, #2813 ) ;
#3970 = CYLINDRICAL_SURFACE ( 'NONE', #5902, 29.99999999999999289 ) ;
#3971 = LINE ( 'NONE', #2756, #5663 ) ;
#3972 = DIRECTION ( 'NONE',  ( -0.000000000000000000, -0.000000000000000000, 1.000000000000000000 ) ) ;
#3973 = ORIENTED_EDGE ( 'NONE', *, *, #4037, .F. ) ;
#3974 = EDGE_CURVE ( 'NONE', #1611, #3001, #4922, .T. ) ;
#3975 = EDGE_LOOP ( 'NONE', ( #6707, #3483, #2366, #3516 ) ) ;
#3976 = AXIS2_PLACEMENT_3D ( 'NONE', #2858, #7622, #3525 ) ;
#3977 = ORIENTED_EDGE ( 'NONE', *, *, #2792, .T. ) ;
#3978 = EDGE_CURVE ( 'NONE', #2537, #578, #3666, .T. ) ;
#3979 = CARTESIAN_POINT ( 'NONE',  ( -73.76644452187066747, 49.96174644486002592, 24.17200000000001125 ) ) ;
#3980 = ADVANCED_FACE ( 'NONE', ( #6742 ), #2543, .T. ) ;
#3981 = DIRECTION ( 'NONE',  ( 1.000000000000000000, 0.000000000000000000, -0.000000000000000000 ) ) ;
#3982 = AXIS2_PLACEMENT_3D ( 'NONE', #4426, #3247, #2583 ) ;
#3983 = CARTESIAN_POINT ( 'NONE',  ( 0.000000000000000000, 150.0000000000000568, 10.00000000000000000 ) ) ;
#3984 = ORIENTED_EDGE ( 'NONE', *, *, #3440, .T. ) ;
#3985 = EDGE_CURVE ( 'NONE', #5419, #3392, #6111, .T. ) ;
#3986 = AXIS2_PLACEMENT_3D ( 'NONE', #5802, #6516, #1105 ) ;
#3987 = DIRECTION ( 'NONE',  ( 0.000000000000000000, 0.000000000000000000, -1.000000000000000000 ) ) ;
#3988 = LINE ( 'NONE', #3364, #7235 ) ;
#3989 = FACE_OUTER_BOUND ( 'NONE', #2959, .T. ) ;
#3990 = CARTESIAN_POINT ( 'NONE',  ( -5.355005115540898863, -6.145890662064660503, -4.617753204360282915 ) ) ;
#3991 = ORIENTED_EDGE ( 'NONE', *, *, #6887, .F. ) ;
#3992 = VECTOR ( 'NONE', #249, 1000.000000000000114 ) ;
#3993 = CARTESIAN_POINT ( 'NONE',  ( 0.000000000000000000, 1.484218055610305731, -3.000000000000000000 ) ) ;
#3994 = FILL_AREA_STYLE ('',( #3444 ) ) ;
#3995 = AXIS2_PLACEMENT_3D ( 'NONE', #793, #2073, #6247 ) ;
#3996 = CARTESIAN_POINT ( 'NONE',  ( 3.200000000000007727, 3.710679801416480038E-15, 30.30000000000000071 ) ) ;
#3997 = CARTESIAN_POINT ( 'NONE',  ( 350.0000000000000000, 300.0000000000000000, -1041.954445729288636 ) ) ;
#3998 = DIRECTION ( 'NONE',  ( -0.000000000000000000, -0.000000000000000000, 1.000000000000000000 ) ) ;
#3999 = ITEM_DEFINED_TRANSFORMATION ( 'NONE', 'NONE', #6625,  #7485 ) ;
#4000 = DIRECTION ( 'NONE',  ( -0.000000000000000000, -0.000000000000000000, 1.000000000000000000 ) ) ;
#4001 = EDGE_LOOP ( 'NONE', ( #5720, #1441, #6580, #3929 ) ) ;
#4002 = VERTEX_POINT ( 'NONE', #7295 ) ;
#4003 = VECTOR ( 'NONE', #7615, 1000.000000000000114 ) ;
#4004 = ORIENTED_EDGE ( 'NONE', *, *, #2362, .F. ) ;
#4005 = CARTESIAN_POINT ( 'NONE',  ( 4.680456609903971277, 6.535341423375591319, -4.683111142572234264 ) ) ;
#4006 = CIRCLE ( 'NONE', #737, 28.49999999999999645 ) ;
#4007 = DIRECTION ( 'NONE',  ( 0.000000000000000000, 0.000000000000000000, -1.000000000000000000 ) ) ;
#4008 = CARTESIAN_POINT ( 'NONE',  ( -68.76644452187072432, 49.96174644486006855, -40.00000000000000000 ) ) ;
#4009 = VECTOR ( 'NONE', #2915, 1000.000000000000000 ) ;
#4010 = DIRECTION ( 'NONE',  ( 1.000000000000000000, 0.000000000000000000, 0.000000000000000000 ) ) ;
#4011 = CYLINDRICAL_SURFACE ( 'NONE', #1755, 32.81578194438969120 ) ;
#4012 = ORIENTED_EDGE ( 'NONE', *, *, #6127, .T. ) ;
#4013 = AXIS2_PLACEMENT_3D ( 'NONE', #607, #684, #7314 ) ;
#4014 = ORIENTED_EDGE ( 'NONE', *, *, #6583, .F. ) ;
#4015 = ORIENTED_EDGE ( 'NONE', *, *, #1914, .T. ) ;
#4016 = DIRECTION ( 'NONE',  ( -0.000000000000000000, -0.000000000000000000, 1.000000000000000000 ) ) ;
#4017 = SURFACE_STYLE_USAGE ( .BOTH. , #6237 ) ;
#4018 = AXIS2_PLACEMENT_3D ( 'NONE', #183, #5507, #6733 ) ;
#4019 = LINE ( 'NONE', #4096, #792 ) ;
#4020 = EDGE_CURVE ( 'NONE', #2474, #2413, #7215, .T. ) ;
#4021 = CARTESIAN_POINT ( 'NONE',  ( -10.00000000000000000, 0.000000000000000000, 10.00000000000000000 ) ) ;
#4022 = ORIENTED_EDGE ( 'NONE', *, *, #2781, .F. ) ;
#4023 = COLOUR_RGB ( '',0.8941176470588234615, 0.8941176470588234615, 0.8941176470588234615 ) ;
#4024 = EDGE_CURVE ( 'NONE', #7389, #3153, #1, .T. ) ;
#4025 = DIRECTION ( 'NONE',  ( 1.000000000000000000, 0.000000000000000000, 0.000000000000000000 ) ) ;
#4026 = CYLINDRICAL_SURFACE ( 'NONE', #7190, 4.250000000000000000 ) ;
#4027 = DIRECTION ( 'NONE',  ( -0.000000000000000000, -0.000000000000000000, -1.000000000000000000 ) ) ;
#4028 = CARTESIAN_POINT ( 'NONE',  ( 26.26644452187053957, 80.83980388508807380, 10.00000000000000000 ) ) ;
#4029 = EDGE_CURVE ( 'NONE', #3857, #1907, #3170, .T. ) ;
#4030 = ORIENTED_EDGE ( 'NONE', *, *, #5811, .T. ) ;
#4031 = ORIENTED_EDGE ( 'NONE', *, *, #6303, .F. ) ;
#4032 = ADVANCED_FACE ( 'NONE', ( #4806 ), #3157, .F. ) ;
#4033 = DIRECTION ( 'NONE',  ( -1.000000000000000000, 0.000000000000000000, 0.000000000000000000 ) ) ;
#4034 = CARTESIAN_POINT ( 'NONE',  ( 0.000000000000000000, 0.000000000000000000, 0.000000000000000000 ) ) ;
#4035 = CARTESIAN_POINT ( 'NONE',  ( -35.00000000000000711, 0.000000000000000000, -50.00000000000000000 ) ) ;
#4036 = DIRECTION ( 'NONE',  ( 0.5000000000000006661, 0.8660254037844383745, -0.000000000000000000 ) ) ;
#4037 = EDGE_CURVE ( 'NONE', #7515, #2283, #5804, .T. ) ;
#4038 = CARTESIAN_POINT ( 'NONE',  ( 0.000000000000000000, 0.000000000000000000, 0.000000000000000000 ) ) ;
#4039 = ORIENTED_EDGE ( 'NONE', *, *, #4403, .T. ) ;
#4040 = ORIENTED_EDGE ( 'NONE', *, *, #4517, .F. ) ;
#4041 = ORIENTED_EDGE ( 'NONE', *, *, #2890, .F. ) ;
#4042 = EDGE_CURVE ( 'NONE', #886, #5665, #4420, .T. ) ;
#4043 = CARTESIAN_POINT ( 'NONE',  ( -1.677050983124841466, 0.000000000000000000, -32.25000000000000000 ) ) ;
#4044 = DIRECTION ( 'NONE',  ( -0.000000000000000000, -0.000000000000000000, -1.000000000000000000 ) ) ;
#4045 = CYLINDRICAL_SURFACE ( 'NONE', #7278, 5.249999999999976907 ) ;
#4046 = CARTESIAN_POINT ( 'NONE',  ( 0.000000000000000000, 0.000000000000000000, -50.00000000000000000 ) ) ;
#4047 = FACE_OUTER_BOUND ( 'NONE', #1133, .T. ) ;
#4048 = ORIENTED_EDGE ( 'NONE', *, *, #4801, .T. ) ;
#4049 = ORIENTED_EDGE ( 'NONE', *, *, #6490, .F. ) ;
#4050 = ORIENTED_EDGE ( 'NONE', *, *, #4507, .F. ) ;
#4051 = CYLINDRICAL_SURFACE ( 'NONE', #3665, 5.249999999999976907 ) ;
#4052 = DIRECTION ( 'NONE',  ( -0.000000000000000000, -0.000000000000000000, -1.000000000000000000 ) ) ;
#4053 =( NAMED_UNIT ( * ) PLANE_ANGLE_UNIT ( ) SI_UNIT ( $, .RADIAN. ) );
#4054 = CARTESIAN_POINT ( 'NONE',  ( 0.000000000000000000, 0.000000000000000000, 0.000000000000000000 ) ) ;
#4055 = DIRECTION ( 'NONE',  ( -0.000000000000000000, -0.000000000000000000, 1.000000000000000000 ) ) ;
#4056 = ORIENTED_EDGE ( 'NONE', *, *, #3471, .F. ) ;
#4057 = ORIENTED_EDGE ( 'NONE', *, *, #5132, .F. ) ;
#4058 = AXIS2_PLACEMENT_3D ( 'NONE', #199, #2616, #6241 ) ;
#4059 = PRODUCT_DEFINITION_CONTEXT ( 'detailed design', #2547, 'design' ) ;
#4060 = CARTESIAN_POINT ( 'NONE',  ( -4.494751301858288528, -36.47409643479112162, -3.000000000000000000 ) ) ;
#4061 = DIRECTION ( 'NONE',  ( 0.5000000000000101030, -0.8660254037844328234, 0.000000000000000000 ) ) ;
#4062 = DIRECTION ( 'NONE',  ( 0.000000000000000000, 0.000000000000000000, 1.000000000000000000 ) ) ;
#4063 = AXIS2_PLACEMENT_3D ( 'NONE', #1249, #6071, #3152 ) ;
#4064 = CYLINDRICAL_SURFACE ( 'NONE', #1666, 5.249999999999976907 ) ;
#4065 = ORIENTED_EDGE ( 'NONE', *, *, #6397, .T. ) ;
#4066 = EDGE_LOOP ( 'NONE', ( #4773, #7151 ) ) ;
#4067 = EDGE_CURVE ( 'NONE', #4638, #502, #5432, .T. ) ;
#4068 = FACE_OUTER_BOUND ( 'NONE', #244, .T. ) ;
#4069 = AXIS2_PLACEMENT_3D ( 'NONE', #7351, #3395, #385 ) ;
#4070 = DIRECTION ( 'NONE',  ( 1.000000000000000000, 0.000000000000000000, 0.000000000000000000 ) ) ;
#4071 = EDGE_CURVE ( 'NONE', #7551, #7307, #4923, .T. ) ;
#4072 = EDGE_CURVE ( 'NONE', #589, #4189, #3049, .T. ) ;
#4073 = DIRECTION ( 'NONE',  ( 1.000000000000000000, 0.000000000000000000, 0.000000000000000000 ) ) ;
#4074 = CYLINDRICAL_SURFACE ( 'NONE', #6168, 5.000000000000004441 ) ;
#4075 = DIRECTION ( 'NONE',  ( 1.000000000000000000, 0.000000000000000000, 0.000000000000000000 ) ) ;
#4076 = ADVANCED_FACE ( 'NONE', ( #6151 ), #5475, .F. ) ;
#4077 = CARTESIAN_POINT ( 'NONE',  ( -6.873268260756527152E-15, 0.000000000000000000, -79.99999999999995737 ) ) ;
#4078 = AXIS2_PLACEMENT_3D ( 'NONE', #2252, #5789, #6578 ) ;
#4079 = EDGE_LOOP ( 'NONE', ( #3245, #2713, #2365, #6322 ) ) ;
#4080 = AXIS2_PLACEMENT_3D ( 'NONE', #4588, #442, #398 ) ;
#4081 = VERTEX_POINT ( 'NONE', #6702 ) ;
#4082 = ORIENTED_EDGE ( 'NONE', *, *, #6879, .F. ) ;
#4083 = CARTESIAN_POINT ( 'NONE',  ( -4.000000000000004441, 6.928203230275506108, 0.000000000000000000 ) ) ;
#4084 = EDGE_CURVE ( 'NONE', #3054, #1983, #640, .T. ) ;
#4085 = LINE ( 'NONE', #6422, #859 ) ;
#4086 = DIRECTION ( 'NONE',  ( 0.000000000000000000, 0.000000000000000000, 1.000000000000000000 ) ) ;
#4087 = DIRECTION ( 'NONE',  ( 0.000000000000000000, 0.000000000000000000, -1.000000000000000000 ) ) ;
#4088 = PLANE ( 'NONE',  #6354 ) ;
#4089 = CARTESIAN_POINT ( 'NONE',  ( 105.4635834177251326, -106.6650485055556601, 5.000000000000000000 ) ) ;
#4090 = EDGE_LOOP ( 'NONE', ( #1402, #3897, #2218, #342 ) ) ;
#4091 = STYLED_ITEM ( 'NONE', ( #7297 ), #4435 ) ;
#4092 = ORIENTED_EDGE ( 'NONE', *, *, #6844, .F. ) ;
#4093 = VERTEX_POINT ( 'NONE', #1978 ) ;
#4094 = CARTESIAN_POINT ( 'NONE',  ( -8.000000000000000000, 0.000000000000000000, -4.700000000000000178 ) ) ;
#4095 = DIRECTION ( 'NONE',  ( 1.000000000000000000, 0.000000000000000000, 0.000000000000000000 ) ) ;
#4096 = CARTESIAN_POINT ( 'NONE',  ( -4.432034252711344102, 28.15327818181735964, -79.99999999999995737 ) ) ;
#4097 = CARTESIAN_POINT ( 'NONE',  ( -1.499999999999999334, -33.63777638310832430, -3.000000000000000000 ) ) ;
#4098 = ORIENTED_EDGE ( 'NONE', *, *, #6595, .T. ) ;
#4099 = VECTOR ( 'NONE', #5102, 1000.000000000000000 ) ;
#4100 = CARTESIAN_POINT ( 'NONE',  ( -2.081668171172168513E-14, -9.237604307034017026, -0.7145311798163319628 ) ) ;
#4101 = DIRECTION ( 'NONE',  ( -0.000000000000000000, -0.000000000000000000, -1.000000000000000000 ) ) ;
#4102 = CIRCLE ( 'NONE', #452, 29.99999999999999289 ) ;
#4103 = DIRECTION ( 'NONE',  ( 5.551115123125782702E-17, 0.000000000000000000, 1.000000000000000000 ) ) ;
#4104 = CYLINDRICAL_SURFACE ( 'NONE', #5691, 31.52499999999999858 ) ;
#4105 = ORIENTED_EDGE ( 'NONE', *, *, #4384, .T. ) ;
#4106 = ORIENTED_EDGE ( 'NONE', *, *, #1835, .T. ) ;
#4107 = CIRCLE ( 'NONE', #4742, 0.3000000000000016542 ) ;
#4108 = DIRECTION ( 'NONE',  ( -0.000000000000000000, -0.000000000000000000, -1.000000000000000000 ) ) ;
#4109 = DIRECTION ( 'NONE',  ( 1.000000000000000000, 0.000000000000000000, 0.000000000000000000 ) ) ;
#4110 = CARTESIAN_POINT ( 'NONE',  ( 129.9038105676665396, -74.99999999999882050, 10.00000000000000000 ) ) ;
#4111 = CARTESIAN_POINT ( 'NONE',  ( -8.000000000000000000, 0.000000000000000000, -4.700000000000000178 ) ) ;
#4112 = LINE ( 'NONE', #7118, #5410 ) ;
#4113 = LINE ( 'NONE', #2821, #6023 ) ;
#4114 = VECTOR ( 'NONE', #6576, 1000.000000000000000 ) ;
#4115 = CYLINDRICAL_SURFACE ( 'NONE', #2206, 10.00000000000000178 ) ;
#4116 = VERTEX_POINT ( 'NONE', #5115 ) ;
#4117 = EDGE_LOOP ( 'NONE', ( #7441, #7091, #2297, #3041 ) ) ;
#4118 = ORIENTED_EDGE ( 'NONE', *, *, #5777, .F. ) ;
#4119 = VECTOR ( 'NONE', #5649, 1000.000000000000000 ) ;
#4120 = EDGE_CURVE ( 'NONE', #4531, #1496, #3672, .T. ) ;
#4121 = PLANE ( 'NONE',  #1654 ) ;
#4122 = CYLINDRICAL_SURFACE ( 'NONE', #4892, 5.857142857142855874 ) ;
#4123 = DIRECTION ( 'NONE',  ( -1.000000000000000000, -0.000000000000000000, -0.000000000000000000 ) ) ;
#4124 = DIRECTION ( 'NONE',  ( 0.4559007153543473412, 0.8900306386520602242, -2.550145071705742900E-17 ) ) ;
#4125 = SURFACE_STYLE_USAGE ( .BOTH. , #2213 ) ;
#4126 = LINE ( 'NONE', #7716, #4009 ) ;
#4127 = AXIS2_PLACEMENT_3D ( 'NONE', #5415, #4854, #7344 ) ;
#4128 = ADVANCED_FACE ( 'NONE', ( #1527 ), #6191, .T. ) ;
#4129 = ORIENTED_EDGE ( 'NONE', *, *, #3264, .F. ) ;
#4130 = ORIENTED_EDGE ( 'NONE', *, *, #1738, .T. ) ;
#4131 = ORIENTED_EDGE ( 'NONE', *, *, #4412, .T. ) ;
#4132 = CIRCLE ( 'NONE', #345, 40.00000000000001421 ) ;
#4133 = DIRECTION ( 'NONE',  ( 1.000000000000000000, 0.000000000000000000, 0.000000000000000000 ) ) ;
#4134 = DIRECTION ( 'NONE',  ( -0.000000000000000000, -0.000000000000000000, -1.000000000000000000 ) ) ;
#4135 =( NAMED_UNIT ( * ) PLANE_ANGLE_UNIT ( ) SI_UNIT ( $, .RADIAN. ) );
#4136 = FACE_OUTER_BOUND ( 'NONE', #6460, .T. ) ;
#4137 = AXIS2_PLACEMENT_3D ( 'NONE', #729, #3577, #6654 ) ;
#4138 = EDGE_CURVE ( 'NONE', #5285, #6434, #1908, .T. ) ;
#4139 = EDGE_LOOP ( 'NONE', ( #1760, #450 ) ) ;
#4140 = ADVANCED_FACE ( 'NONE', ( #6859, #891 ), #6899, .F. ) ;
#4141 = VECTOR ( 'NONE', #3961, 1000.000000000000000 ) ;
#4142 = FACE_OUTER_BOUND ( 'NONE', #7224, .T. ) ;
#4143 = DIRECTION ( 'NONE',  ( 0.000000000000000000, 0.000000000000000000, -1.000000000000000000 ) ) ;
#4144 =( REPRESENTATION_RELATIONSHIP ('NONE','NONE', #1229, #420 ) REPRESENTATION_RELATIONSHIP_WITH_TRANSFORMATION ( #4827 )SHAPE_REPRESENTATION_RELATIONSHIP( ) );
#4145 = DIRECTION ( 'NONE',  ( 0.000000000000000000, 0.000000000000000000, -1.000000000000000000 ) ) ;
#4146 = CARTESIAN_POINT ( 'NONE',  ( 85.00000000000000000, 9.720002580593245511E-13, 10.00000000000000000 ) ) ;
#4147 = ORIENTED_EDGE ( 'NONE', *, *, #426, .T. ) ;
#4148 = AXIS2_PLACEMENT_3D ( 'NONE', #2489, #3816, #4876 ) ;
#4149 = EDGE_LOOP ( 'NONE', ( #4848, #504 ) ) ;
#4150 = EDGE_LOOP ( 'NONE', ( #3417, #5360, #7292, #2617 ) ) ;
#4151 =( NAMED_UNIT ( * ) PLANE_ANGLE_UNIT ( ) SI_UNIT ( $, .RADIAN. ) );
#4152 = DIRECTION ( 'NONE',  ( 0.000000000000000000, 0.000000000000000000, -1.000000000000000000 ) ) ;
#4153 = VECTOR ( 'NONE', #4735, 1000.000000000000000 ) ;
#4154 = CARTESIAN_POINT ( 'NONE',  ( 3.199999999999996181, 0.000000000000000000, -37.19999999999999574 ) ) ;
#4155 = CARTESIAN_POINT ( 'NONE',  ( -125.2481648402875578, 207.8429183184017859, -120.0000000000000000 ) ) ;
#4156 = CARTESIAN_POINT ( 'NONE',  ( 114.7481648402866341, 207.8429183184022122, -50.00000000000000000 ) ) ;
#4157 = ITEM_DEFINED_TRANSFORMATION ( 'NONE', 'NONE', #1201,  #7485 ) ;
#4158 = CARTESIAN_POINT ( 'NONE',  ( 3.499999999999996003, 0.000000000000000000, 0.000000000000000000 ) ) ;
#4159 = ORIENTED_EDGE ( 'NONE', *, *, #2735, .F. ) ;
#4160 = VERTEX_POINT ( 'NONE', #3782 ) ;
#4161 = PRODUCT_DEFINITION ( 'UNKNOWN', '', #5069, #4492 ) ;
#4162 = CARTESIAN_POINT ( 'NONE',  ( 7.347286611336970807, 4.995646404165279719, -4.203039949738250236 ) ) ;
#4163 = LINE ( 'NONE', #4204, #1882 ) ;
#4164 = CARTESIAN_POINT ( 'NONE',  ( -3.499999999999996003, 0.000000000000000000, -37.19999999999999574 ) ) ;
#4165 = CARTESIAN_POINT ( 'NONE',  ( 207.8429183184022122, 119.9981648402868331, 14.70000000000000462 ) ) ;
#4166 = AXIS2_PLACEMENT_3D ( 'NONE', #2686, #6275, #3944 ) ;
#4167 = DIRECTION ( 'NONE',  ( -0.000000000000000000, -0.000000000000000000, 1.000000000000000000 ) ) ;
#4168 = DIRECTION ( 'NONE',  ( -0.000000000000000000, -0.000000000000000000, -1.000000000000000000 ) ) ;
#4169 = VERTEX_POINT ( 'NONE', #854 ) ;
#4170 = ORIENTED_EDGE ( 'NONE', *, *, #7204, .F. ) ;
#4171 = EDGE_CURVE ( 'NONE', #7537, #926, #776, .T. ) ;
#4172 = ORIENTED_EDGE ( 'NONE', *, *, #6211, .T. ) ;
#4173 = CARTESIAN_POINT ( 'NONE',  ( -8.000000000000000000, 3.871967595402128648, -4.201061386767543482 ) ) ;
#4174 = DIRECTION ( 'NONE',  ( -0.000000000000000000, -0.000000000000000000, 1.000000000000000000 ) ) ;
#4175 = ADVANCED_FACE ( 'NONE', ( #6784 ), #189, .T. ) ;
#4176 = SURFACE_SIDE_STYLE ('',( #5408 ) ) ;
#4177 = EDGE_CURVE ( 'NONE', #5419, #115, #2295, .T. ) ;
#4178 = DIRECTION ( 'NONE',  ( 1.000000000000000000, 0.000000000000000000, 0.000000000000000000 ) ) ;
#4179 = EDGE_CURVE ( 'NONE', #1026, #980, #4486, .T. ) ;
#4180 = ORIENTED_EDGE ( 'NONE', *, *, #1691, .F. ) ;
#4181 = ORIENTED_EDGE ( 'NONE', *, *, #3907, .T. ) ;
#4182 = AXIS2_PLACEMENT_3D ( 'NONE', #2662, #1426, #1469 ) ;
#4183 = EDGE_CURVE ( 'NONE', #5921, #6833, #2664, .T. ) ;
#4184 = FACE_OUTER_BOUND ( 'NONE', #5781, .T. ) ;
#4185 = VECTOR ( 'NONE', #99, 1000.000000000000000 ) ;
#4186 = DIRECTION ( 'NONE',  ( -0.000000000000000000, -0.000000000000000000, 1.000000000000000000 ) ) ;
#4187 = CARTESIAN_POINT ( 'NONE',  ( 31.51644452187122525, -80.83980388508783221, 10.00000000000000000 ) ) ;
#4188 = CIRCLE ( 'NONE', #5956, 32.81578194438969120 ) ;
#4189 = VERTEX_POINT ( 'NONE', #4447 ) ;
#4190 = DIRECTION ( 'NONE',  ( -0.000000000000000000, -0.000000000000000000, 1.000000000000000000 ) ) ;
#4191 = VERTEX_POINT ( 'NONE', #299 ) ;
#4192 = ORIENTED_EDGE ( 'NONE', *, *, #2735, .T. ) ;
#4193 = FACE_OUTER_BOUND ( 'NONE', #1653, .T. ) ;
#4194 = CARTESIAN_POINT ( 'NONE',  ( 0.000000000000000000, 0.000000000000000000, 10.00000000000000000 ) ) ;
#4195 = AXIS2_PLACEMENT_3D ( 'NONE', #4194, #1799, #4602 ) ;
#4196 = CARTESIAN_POINT ( 'NONE',  ( 145.1064334105738567, -38.00161816110872337, 0.000000000000000000 ) ) ;
#4197 = CARTESIAN_POINT ( 'NONE',  ( -3.199999999999994404, 0.000000000000000000, 0.000000000000000000 ) ) ;
#4198 = CONTEXT_DEPENDENT_SHAPE_REPRESENTATION ( #3199, #6051 ) ;
#4199 = DIRECTION ( 'NONE',  ( -0.000000000000000000, -0.000000000000000000, 1.000000000000000000 ) ) ;
#4200 = VERTEX_POINT ( 'NONE', #2607 ) ;
#4201 = EDGE_LOOP ( 'NONE', ( #424, #5306, #7023, #2256 ) ) ;
#4202 = CONICAL_SURFACE ( 'NONE', #1303, 4.999999999999990230, 0.7853981633974482790 ) ;
#4203 = CARTESIAN_POINT ( 'NONE',  ( -119.9981648402868046, 207.8429183184021554, 10.00000000000000178 ) ) ;
#4204 = CARTESIAN_POINT ( 'NONE',  ( -5.000000000000000888, 0.000000000000000000, -4.674599999999997202 ) ) ;
#4205 = CARTESIAN_POINT ( 'NONE',  ( -73.76644452187068168, 49.96174644486002592, 0.000000000000000000 ) ) ;
#4206 = DIRECTION ( 'NONE',  ( 0.3090169943749582204, -0.9510565162951500895, 0.000000000000000000 ) ) ;
#4207 = CIRCLE ( 'NONE', #297, 10.00000000000000178 ) ;
#4208 = DIRECTION ( 'NONE',  ( 1.000000000000000000, 0.000000000000000000, 0.000000000000000000 ) ) ;
#4209 = DIRECTION ( 'NONE',  ( -1.000000000000000000, 0.000000000000000000, 0.000000000000000000 ) ) ;
#4210 = ORIENTED_EDGE ( 'NONE', *, *, #5132, .T. ) ;
#4211 = ORIENTED_EDGE ( 'NONE', *, *, #768, .F. ) ;
#4212 = CIRCLE ( 'NONE', #5090, 29.99999999999999289 ) ;
#4213 = ORIENTED_EDGE ( 'NONE', *, *, #6873, .T. ) ;
#4214 = DIRECTION ( 'NONE',  ( 1.000000000000000000, 0.000000000000000000, 0.000000000000000000 ) ) ;
#4215 = DIRECTION ( 'NONE',  ( 1.000000000000000000, 0.000000000000000000, 0.000000000000000000 ) ) ;
#4216 = CARTESIAN_POINT ( 'NONE',  ( 5.870234470492294880E-31, -4.203179568131150526E-15, -122.9999999999999716 ) ) ;
#4217 = AXIS2_PLACEMENT_3D ( 'NONE', #3531, #532, #2946 ) ;
#4218 = ADVANCED_FACE ( 'NONE', ( #7443 ), #6823, .F. ) ;
#4219 = PRODUCT_DEFINITION_SHAPE ( 'NONE', 'NONE',  #7774 ) ;
#4220 = EDGE_LOOP ( 'NONE', ( #3283, #1893, #5961 ) ) ;
#4221 = VERTEX_POINT ( 'NONE', #5634 ) ;
#4222 = AXIS2_PLACEMENT_3D ( 'NONE', #5989, #5398, #1283 ) ;
#4223 = EDGE_CURVE ( 'NONE', #5913, #3506, #1269, .T. ) ;
#4224 = CARTESIAN_POINT ( 'NONE',  ( 0.000000000000000000, 0.000000000000000000, -139.9999999999999716 ) ) ;
#4225 = CARTESIAN_POINT ( 'NONE',  ( 0.000000000000000000, 0.000000000000000000, -139.9999999999999716 ) ) ;
#4226 = FACE_OUTER_BOUND ( 'NONE', #148, .T. ) ;
#4227 = ORIENTED_EDGE ( 'NONE', *, *, #3700, .F. ) ;
#4228 = EDGE_CURVE ( 'NONE', #2556, #7599, #7065, .T. ) ;
#4229 = ORIENTED_EDGE ( 'NONE', *, *, #6959, .F. ) ;
#4230 = AXIS2_PLACEMENT_3D ( 'NONE', #1962, #3184, #6772 ) ;
#4231 = CARTESIAN_POINT ( 'NONE',  ( -5.846731056662409998, 29.42474699893032763, -139.9999999999999716 ) ) ;
#4232 = PLANE ( 'NONE',  #4960 ) ;
#4233 = LINE ( 'NONE', #7156, #1369 ) ;
#4234 = CARTESIAN_POINT ( 'NONE',  ( 119.9981648402866341, 207.8429183184022122, -50.00000000000000000 ) ) ;
#4235 = CONTEXT_DEPENDENT_SHAPE_REPRESENTATION ( #3598, #6117 ) ;
#4236 = UNCERTAINTY_MEASURE_WITH_UNIT (LENGTH_MEASURE( 1.000000000000000082E-05 ), #6039, 'distance_accuracy_value', 'NONE');
#4237 = FACE_OUTER_BOUND ( 'NONE', #7378, .T. ) ;
#4238 = EDGE_LOOP ( 'NONE', ( #449, #4213, #4326, #2791 ) ) ;
#4239 = DIRECTION ( 'NONE',  ( -0.000000000000000000, -0.000000000000000000, 1.000000000000000000 ) ) ;
#4240 = EDGE_CURVE ( 'NONE', #6357, #7233, #6694, .T. ) ;
#4241 = AXIS2_PLACEMENT_3D ( 'NONE', #4665, #7577, #7661 ) ;
#4242 = DIRECTION ( 'NONE',  ( -0.000000000000000000, -0.000000000000000000, 1.000000000000000000 ) ) ;
#4243 = FACE_OUTER_BOUND ( 'NONE', #4304, .T. ) ;
#4244 = DIRECTION ( 'NONE',  ( -0.9987587364483918595, -0.04980950078059115382, 0.000000000000000000 ) ) ;
#4245 = CARTESIAN_POINT ( 'NONE',  ( 3.500000000000006661, 0.000000000000000000, 0.000000000000000000 ) ) ;
#4246 = DIRECTION ( 'NONE',  ( -0.000000000000000000, -0.000000000000000000, 1.000000000000000000 ) ) ;
#4247 = PLANE ( 'NONE',  #4572 ) ;
#4248 = ORIENTED_EDGE ( 'NONE', *, *, #1747, .T. ) ;
#4249 = VECTOR ( 'NONE', #4832, 1000.000000000000000 ) ;
#4250 = ORIENTED_EDGE ( 'NONE', *, *, #768, .T. ) ;
#4251 = VERTEX_POINT ( 'NONE', #6308 ) ;
#4252 = DIRECTION ( 'NONE',  ( -0.000000000000000000, -0.000000000000000000, 1.000000000000000000 ) ) ;
#4253 = SURFACE_SIDE_STYLE ('',( #75 ) ) ;
#4254 = AXIS2_PLACEMENT_3D ( 'NONE', #2361, #4747, #7157 ) ;
#4255 = CARTESIAN_POINT ( 'NONE',  ( -8.000000000000000000, -4.618802153517013842, -0.7145311798163319628 ) ) ;
#4256 = EDGE_LOOP ( 'NONE', ( #3712, #4782, #2877, #4791 ) ) ;
#4257 = VERTEX_POINT ( 'NONE', #2134 ) ;
#4258 = AXIS2_PLACEMENT_3D ( 'NONE', #4225, #2972, #6637 ) ;
#4259 = EDGE_CURVE ( 'NONE', #3942, #6304, #4525, .T. ) ;
#4260 = CARTESIAN_POINT ( 'NONE',  ( -1.728922298134113098E-15, 8.513302795252935035E-16, 10.00000000000000000 ) ) ;
#4261 = AXIS2_PLACEMENT_3D ( 'NONE', #4988, #1357, #5657 ) ;
#4262 = CARTESIAN_POINT ( 'NONE',  ( -2.645508037661889134, -7.710219529346611367, -0.06809871960543237290 ) ) ;
#4263 = CARTESIAN_POINT ( 'NONE',  ( -3.500000000000006661, 3.949485927250214050E-15, 32.25000000000000000 ) ) ;
#4264 = VERTEX_POINT ( 'NONE', #2755 ) ;
#4265 = AXIS2_PLACEMENT_3D ( 'NONE', #1076, #443, #5142 ) ;
#4266 = EDGE_LOOP ( 'NONE', ( #1928, #6544, #4181, #4882 ) ) ;
#4267 = DIRECTION ( 'NONE',  ( 1.000000000000000000, 0.000000000000000000, 0.000000000000000000 ) ) ;
#4268 = CARTESIAN_POINT ( 'NONE',  ( -10.00000000000000000, 0.000000000000000000, 0.000000000000000000 ) ) ;
#4269 = FACE_BOUND ( 'NONE', #962, .T. ) ;
#4270 = PLANE ( 'NONE',  #6147 ) ;
#4271 = EDGE_CURVE ( 'NONE', #924, #4732, #5153, .T. ) ;
#4272 = CIRCLE ( 'NONE', #4401, 5.249999999999976907 ) ;
#4273 = CARTESIAN_POINT ( 'NONE',  ( -4.000000000000000000, -33.63777638310832430, 0.000000000000000000 ) ) ;
#4274 = ORIENTED_EDGE ( 'NONE', *, *, #4228, .F. ) ;
#4275 = EDGE_CURVE ( 'NONE', #1642, #3671, #2796, .T. ) ;
#4276 = PRESENTATION_LAYER_ASSIGNMENT (  '', '', ( #3402 ) ) ;
#4277 = LINE ( 'NONE', #615, #3189 ) ;
#4278 = EDGE_CURVE ( 'NONE', #3955, #1610, #4704, .T. ) ;
#4279 = DIRECTION ( 'NONE',  ( -0.000000000000000000, -0.000000000000000000, 1.000000000000000000 ) ) ;
#4280 = DIRECTION ( 'NONE',  ( 0.000000000000000000, 0.000000000000000000, 1.000000000000000000 ) ) ;
#4281 = CARTESIAN_POINT ( 'NONE',  ( 5.777789833161707559E-31, -4.119912841284263785E-15, -119.9999999999999716 ) ) ;
#4282 = PRODUCT_DEFINITION_SHAPE ( 'NONE', 'NONE',  #7765 ) ;
#4283 =( LENGTH_UNIT ( ) NAMED_UNIT ( * ) SI_UNIT ( .MILLI., .METRE. ) );
#4284 = DIRECTION ( 'NONE',  ( 0.000000000000000000, 0.000000000000000000, 1.000000000000000000 ) ) ;
#4285 = UNCERTAINTY_MEASURE_WITH_UNIT (LENGTH_MEASURE( 1.000000000000000082E-05 ), #3462, 'distance_accuracy_value', 'NONE');
#4287 = AXIS2_PLACEMENT_3D ( 'NONE', #1338, #120, #5448 ) ;
#4286 = CARTESIAN_POINT ( 'NONE',  ( 2.583028308771596837, 28.38270538120150377, 13.00000000000000178 ) ) ;
#4288 = ADVANCED_FACE ( 'NONE', ( #5903 ), #4122, .F. ) ;
#4289 = ORIENTED_EDGE ( 'NONE', *, *, #7213, .F. ) ;
#4290 = EDGE_LOOP ( 'NONE', ( #860, #1040, #5043, #4804 ) ) ;
#4291 = ORIENTED_EDGE ( 'NONE', *, *, #7359, .F. ) ;
#4292 = VECTOR ( 'NONE', #7566, 1000.000000000000000 ) ;
#4293 = CARTESIAN_POINT ( 'NONE',  ( 129.9038105676665396, -74.99999999999882050, 10.00000000000000000 ) ) ;
#4294 =( NAMED_UNIT ( * ) PLANE_ANGLE_UNIT ( ) SI_UNIT ( $, .RADIAN. ) );
#4295 = CARTESIAN_POINT ( 'NONE',  ( -20.63749999999999574, 0.000000000000000000, 0.000000000000000000 ) ) ;
#4296 = ORIENTED_EDGE ( 'NONE', *, *, #789, .T. ) ;
#4297 = AXIS2_PLACEMENT_3D ( 'NONE', #3234, #259, #3822 ) ;
#4298 = ORIENTED_EDGE ( 'NONE', *, *, #7269, .T. ) ;
#4299 = DIRECTION ( 'NONE',  ( 0.000000000000000000, 0.000000000000000000, 1.000000000000000000 ) ) ;
#4300 = PLANE ( 'NONE',  #1061 ) ;
#4301 = DIRECTION ( 'NONE',  ( -0.000000000000000000, -0.000000000000000000, -1.000000000000000000 ) ) ;
#4302 = DIRECTION ( 'NONE',  ( -0.000000000000000000, -0.000000000000000000, -1.000000000000000000 ) ) ;
#4303 = ORIENTED_EDGE ( 'NONE', *, *, #2219, .F. ) ;
#4304 = EDGE_LOOP ( 'NONE', ( #4130, #2326, #6379, #2793, #3206, #7261, #4672, #4227 ) ) ;
#4305 = CYLINDRICAL_SURFACE ( 'NONE', #4616, 32.25000000000000000 ) ;
#4306 = CARTESIAN_POINT ( 'NONE',  ( 0.000000000000000000, 0.000000000000000000, -82.99999999999995737 ) ) ;
#4307 = CARTESIAN_POINT ( 'NONE',  ( 0.7499999999999730216, -37.49249924984995630, 0.000000000000000000 ) ) ;
#4308 = DIRECTION ( 'NONE',  ( 1.000000000000000000, 0.000000000000000000, 0.000000000000000000 ) ) ;
#4309 = CIRCLE ( 'NONE', #3936, 5.249999999999976907 ) ;
#4310 = CARTESIAN_POINT ( 'NONE',  ( 0.000000000000000000, 4.250000000000000000, 2.573333333332999739 ) ) ;
#4311 = ORIENTED_EDGE ( 'NONE', *, *, #5808, .F. ) ;
#4312 = ADVANCED_FACE ( 'NONE', ( #6538 ), #1604, .F. ) ;
#4313 = ADVANCED_FACE ( 'NONE', ( #4641 ), #5355, .T. ) ;
#4314 = VECTOR ( 'NONE', #5968, 1000.000000000000000 ) ;
#4315 = EDGE_CURVE ( 'NONE', #2582, #5462, #1684, .T. ) ;
#4316 = DIRECTION ( 'NONE',  ( -0.000000000000000000, -0.000000000000000000, 1.000000000000000000 ) ) ;
#4317 = EDGE_CURVE ( 'NONE', #6929, #4081, #4006, .T. ) ;
#4318 = CARTESIAN_POINT ( 'NONE',  ( 3.716043017018883621, 28.25669875083898930, 10.00000000000000000 ) ) ;
#4319 = CARTESIAN_POINT ( 'NONE',  ( -350.0000000000000000, -299.9999999999998863, -120.0000000000000000 ) ) ;
#4320 = SHAPE_DEFINITION_REPRESENTATION ( #1387, #2561 ) ;
#4321 = SURFACE_SIDE_STYLE ('',( #655 ) ) ;
#4322 = LINE ( 'NONE', #733, #6291 ) ;
#4323 = AXIS2_PLACEMENT_3D ( 'NONE', #7289, #623, #6105 ) ;
#4324 = DIRECTION ( 'NONE',  ( 1.000000000000000000, 0.000000000000000000, 0.000000000000000000 ) ) ;
#4325 = ORIENTED_EDGE ( 'NONE', *, *, #7163, .F. ) ;
#4326 = ORIENTED_EDGE ( 'NONE', *, *, #1032, .T. ) ;
#4327 = EDGE_CURVE ( 'NONE', #4116, #2529, #474, .T. ) ;
#4328 = VERTEX_POINT ( 'NONE', #1125 ) ;
#4329 = AXIS2_PLACEMENT_3D ( 'NONE', #3785, #3047, #6114 ) ;
#4330 = DIRECTION ( 'NONE',  ( 0.000000000000000000, 0.000000000000000000, 1.000000000000000000 ) ) ;
#4331 = PRESENTATION_STYLE_ASSIGNMENT (( #7405 ) ) ;
#4332 = DIRECTION ( 'NONE',  ( -3.081487911019577365E-33, 2.775557561562891967E-17, 1.000000000000000000 ) ) ;
#4333 = ORIENTED_EDGE ( 'NONE', *, *, #2110, .T. ) ;
#4334 = AXIS2_PLACEMENT_3D ( 'NONE', #2718, #2644, #6825 ) ;
#4335 = ORIENTED_EDGE ( 'NONE', *, *, #4957, .F. ) ;
#4336 = CIRCLE ( 'NONE', #552, 0.3000000000000016542 ) ;
#4337 = ORIENTED_EDGE ( 'NONE', *, *, #2120, .T. ) ;
#4338 = CARTESIAN_POINT ( 'NONE',  ( 119.9981648402866341, 207.8429183184022122, -50.00000000000000000 ) ) ;
#4340 = VECTOR ( 'NONE', #7667, 1000.000000000000000 ) ;
#4339 = DIRECTION ( 'NONE',  ( 0.000000000000000000, 0.000000000000000000, 1.000000000000000000 ) ) ;
#4341 = DIRECTION ( 'NONE',  ( 2.398081733190337496E-14, 1.000000000000000000, -0.000000000000000000 ) ) ;
#4342 = DIRECTION ( 'NONE',  ( 0.9938725510941108787, -0.1105321318969463978, 0.000000000000000000 ) ) ;
#4343 = ORIENTED_EDGE ( 'NONE', *, *, #3713, .T. ) ;
#4344 = AXIS2_PLACEMENT_3D ( 'NONE', #3347, #2913, #1007 ) ;
#4345 = EDGE_LOOP ( 'NONE', ( #4092, #1791, #15, #3415 ) ) ;
#4346 = PRODUCT_DEFINITION_SHAPE ( 'NONE', 'NONE',  #7788 ) ;
#4347 = CARTESIAN_POINT ( 'NONE',  ( 10.00000000000000000, 0.000000000000000000, -60.00000000000000711 ) ) ;
#4348 = CARTESIAN_POINT ( 'NONE',  ( 125.2481648402868615, 207.8429183184021269, 10.00000000000000000 ) ) ;
#4349 = DIRECTION ( 'NONE',  ( 1.000000000000000000, 0.000000000000000000, 0.000000000000000000 ) ) ;
#4350 = CARTESIAN_POINT ( 'NONE',  ( 3.911624228440929940, 29.74389342193576979, -139.9999999999999716 ) ) ;
#4351 = DIRECTION ( 'NONE',  ( 1.000000000000000000, 0.000000000000000000, 0.000000000000000000 ) ) ;
#4352 = ORIENTED_EDGE ( 'NONE', *, *, #529, .F. ) ;
#4353 = AXIS2_PLACEMENT_3D ( 'NONE', #4203, #651, #690 ) ;
#4354 = CARTESIAN_POINT ( 'NONE',  ( -68.76644452187068168, 49.96174644486002592, 10.00000000000000000 ) ) ;
#4355 = CARTESIAN_POINT ( 'NONE',  ( 350.0000000000000000, 300.0000000000000000, -82.99999999999998579 ) ) ;
#4356 = CARTESIAN_POINT ( 'NONE',  ( 0.000000000000000000, 0.000000000000000000, -119.9999999999999858 ) ) ;
#4357 = FACE_OUTER_BOUND ( 'NONE', #200, .T. ) ;
#4358 = SHAPE_DEFINITION_REPRESENTATION ( #3225, #5012 ) ;
#4359 = AXIS2_PLACEMENT_3D ( 'NONE', #5421, #51, #17 ) ;
#4360 = DIRECTION ( 'NONE',  ( 0.000000000000000000, 0.000000000000000000, -1.000000000000000000 ) ) ;
#4361 = FACE_BOUND ( 'NONE', #7193, .T. ) ;
#4362 = ORIENTED_EDGE ( 'NONE', *, *, #6602, .T. ) ;
#4363 = EDGE_CURVE ( 'NONE', #6304, #4648, #2171, .T. ) ;
#4364 = VERTEX_POINT ( 'NONE', #7593 ) ;
#4365 = CIRCLE ( 'NONE', #3361, 32.49999999999997158 ) ;
#4366 = ORIENTED_EDGE ( 'NONE', *, *, #2209, .F. ) ;
#4367 = CARTESIAN_POINT ( 'NONE',  ( -145.1064334105733451, -38.00161816111073421, 5.000000000000000000 ) ) ;
#4368 = LINE ( 'NONE', #6785, #1129 ) ;
#4369 =( NAMED_UNIT ( * ) PLANE_ANGLE_UNIT ( ) SI_UNIT ( $, .RADIAN. ) );
#4370 = CARTESIAN_POINT ( 'NONE',  ( 10.00000000000000000, 0.000000000000000000, -60.00000000000000711 ) ) ;
#4371 = EDGE_CURVE ( 'NONE', #2263, #3181, #2761, .T. ) ;
#4372 = EDGE_LOOP ( 'NONE', ( #797, #5509, #4609, #7477 ) ) ;
#4373 = ORIENTED_EDGE ( 'NONE', *, *, #6890, .T. ) ;
#4374 = ADVANCED_FACE ( 'NONE', ( #3460 ), #3970, .T. ) ;
#4375 = ORIENTED_EDGE ( 'NONE', *, *, #3927, .F. ) ;
#4376 = UNCERTAINTY_MEASURE_WITH_UNIT (LENGTH_MEASURE( 1.000000000000000082E-05 ), #2343, 'distance_accuracy_value', 'NONE');
#4377 = PLANE ( 'NONE',  #3408 ) ;
#4378 =( NAMED_UNIT ( * ) PLANE_ANGLE_UNIT ( ) SI_UNIT ( $, .RADIAN. ) );
#4379 = EDGE_CURVE ( 'NONE', #1483, #7447, #4085, .T. ) ;
#4380 = CARTESIAN_POINT ( 'NONE',  ( 89.90381056766497636, 75.00000000000153477, 10.00000000000000000 ) ) ;
#4381 = DIRECTION ( 'NONE',  ( 0.000000000000000000, -1.000000000000000000, 0.000000000000000000 ) ) ;
#4382 = EDGE_LOOP ( 'NONE', ( #3085, #2272, #7225, #6249 ) ) ;
#4383 = VECTOR ( 'NONE', #1995, 999.9999999999998863 ) ;
#4384 = EDGE_CURVE ( 'NONE', #5437, #6698, #6282, .T. ) ;
#4385 = CARTESIAN_POINT ( 'NONE',  ( 0.000000000000000000, 1.484218055610305731, -3.000000000000000000 ) ) ;
#4386 = CYLINDRICAL_SURFACE ( 'NONE', #1695, 5.250000000000004441 ) ;
#4387 = VECTOR ( 'NONE', #7011, 1000.000000000000000 ) ;
#4388 = CARTESIAN_POINT ( 'NONE',  ( -10.00000000000000000, 41.99999999999999289, 10.00000000000000000 ) ) ;
#4389 = CARTESIAN_POINT ( 'NONE',  ( 350.0000000000000000, 37.15382499588017140, -120.0000000000000000 ) ) ;
#4390 = ORIENTED_EDGE ( 'NONE', *, *, #6782, .T. ) ;
#4391 = AXIS2_PLACEMENT_3D ( 'NONE', #2181, #6908, #6353 ) ;
#4392 = CARTESIAN_POINT ( 'NONE',  ( -3.199999999999996181, 0.000000000000000000, 0.000000000000000000 ) ) ;
#4393 = FACE_OUTER_BOUND ( 'NONE', #2569, .T. ) ;
#4394 = VECTOR ( 'NONE', #4246, 1000.000000000000000 ) ;
#4395 = DIRECTION ( 'NONE',  ( -1.000000000000000000, 0.000000000000000000, 0.000000000000000000 ) ) ;
#4396 = FACE_OUTER_BOUND ( 'NONE', #6170, .T. ) ;
#4397 = CARTESIAN_POINT ( 'NONE',  ( -74.01644452187068168, 49.96174644486002592, 10.00000000000000000 ) ) ;
#4398 = DIRECTION ( 'NONE',  ( 0.000000000000000000, 0.000000000000000000, 1.000000000000000000 ) ) ;
#4399 = VERTEX_POINT ( 'NONE', #377 ) ;
#4400 = ORIENTED_EDGE ( 'NONE', *, *, #5088, .F. ) ;
#4401 = AXIS2_PLACEMENT_3D ( 'NONE', #7171, #1050, #622 ) ;
#4402 = ORIENTED_EDGE ( 'NONE', *, *, #4896, .F. ) ;
#4403 = EDGE_CURVE ( 'NONE', #1974, #6664, #2393, .T. ) ;
#4404 = ORIENTED_EDGE ( 'NONE', *, *, #5128, .T. ) ;
#4405 = DIRECTION ( 'NONE',  ( 0.000000000000000000, 0.000000000000000000, 1.000000000000000000 ) ) ;
#4406 = DIRECTION ( 'NONE',  ( 0.000000000000000000, 0.000000000000000000, -1.000000000000000000 ) ) ;
#4407 = PRESENTATION_STYLE_ASSIGNMENT (( #820 ) ) ;
#4408 = CIRCLE ( 'NONE', #2532, 5.249999999999987566 ) ;
#4409 = DIRECTION ( 'NONE',  ( 1.000000000000000000, 0.000000000000000000, 0.000000000000000000 ) ) ;
#4410 = PRODUCT_DEFINITION_SHAPE ( 'NONE', 'NONE',  #7773 ) ;
#4411 = EDGE_LOOP ( 'NONE', ( #188, #7565, #1521, #4482, #3327, #6749, #1346, #4445, #1287, #4366, #2602, #7679 ) ) ;
#4412 = EDGE_CURVE ( 'NONE', #3662, #6904, #5017, .T. ) ;
#4413 = EDGE_LOOP ( 'NONE', ( #6261, #3175, #381, #1520, #812, #6225 ) ) ;
#4414 = AXIS2_PLACEMENT_3D ( 'NONE', #43, #2467, #1942 ) ;
#4415 = EDGE_CURVE ( 'NONE', #2423, #719, #2387, .T. ) ;
#4416 = ADVANCED_FACE ( 'NONE', ( #3105, #3690 ), #1773, .T. ) ;
#4417 = DIRECTION ( 'NONE',  ( 1.000000000000000000, 0.000000000000000000, 0.000000000000000000 ) ) ;
#4418 = EDGE_CURVE ( 'NONE', #738, #2609, #7293, .T. ) ;
#4419 = DIRECTION ( 'NONE',  ( -0.000000000000000000, -0.000000000000000000, 1.000000000000000000 ) ) ;
#4420 = CIRCLE ( 'NONE', #1013, 28.50000000000000711 ) ;
#4421 = PLANE ( 'NONE',  #542 ) ;
#4422 = ORIENTED_EDGE ( 'NONE', *, *, #7121, .F. ) ;
#4423 = TOROIDAL_SURFACE ( 'NONE', #3799, 30.30000000000000071, 0.3000000000000003775 ) ;
#4424 = EDGE_CURVE ( 'NONE', #2263, #6942, #6066, .T. ) ;
#4425 = TOROIDAL_SURFACE ( 'NONE', #612, 33.75000000000000000, 2.250000000000000444 ) ;
#4426 = CARTESIAN_POINT ( 'NONE',  ( 2.750000000000000000, -33.63777638310832430, -3.000000000000000000 ) ) ;
#4427 = DIRECTION ( 'NONE',  ( -1.000000000000000000, 0.000000000000000000, 0.000000000000000000 ) ) ;
#4428 = DIRECTION ( 'NONE',  ( 0.000000000000000000, 0.000000000000000000, -1.000000000000000000 ) ) ;
#4429 = DIRECTION ( 'NONE',  ( 1.000000000000000000, 0.000000000000000000, 0.000000000000000000 ) ) ;
#4430 = B_SPLINE_CURVE_WITH_KNOTS ( 'NONE', 3,
 ( #2248, #6535, #536, #410, #2286, #4083 ),
 .UNSPECIFIED., .F., .F.,
 ( 4, 2, 4 ),
 ( 2.380731629582122378E-07, 0.002336973833157555969, 0.004673709593152153112 ),
 .UNSPECIFIED. ) ;
#4431 = ORIENTED_EDGE ( 'NONE', *, *, #4177, .F. ) ;
#4432 = DIRECTION ( 'NONE',  ( 0.9412010056177179118, 0.3378471059875997051, 1.703375277368107492E-17 ) ) ;
#4433 = LINE ( 'NONE', #2593, #7496 ) ;
#4434 = CIRCLE ( 'NONE', #1024, 5.250000000000004441 ) ;
#4435 = ADVANCED_BREP_SHAPE_REPRESENTATION ( '', ( #525, #7485 ), #4585 ) ;
#4436 = DIRECTION ( 'NONE',  ( -0.000000000000000000, -0.000000000000000000, 1.000000000000000000 ) ) ;
#4437 = CARTESIAN_POINT ( 'NONE',  ( -78.76644452187068168, 49.96174644486002592, -40.00000000000000000 ) ) ;
#4438 = DIRECTION ( 'NONE',  ( 0.000000000000000000, 0.000000000000000000, 1.000000000000000000 ) ) ;
#4439 = CARTESIAN_POINT ( 'NONE',  ( 9.702951051037011609, -29.86427928513813868, -3.000000000000000000 ) ) ;
#4440 = DIRECTION ( 'NONE',  ( -0.000000000000000000, -0.000000000000000000, 1.000000000000000000 ) ) ;
#4441 = ORIENTED_EDGE ( 'NONE', *, *, #3026, .T. ) ;
#4442 = ORIENTED_EDGE ( 'NONE', *, *, #668, .F. ) ;
#4443 = VECTOR ( 'NONE', #2887, 1000.000000000000000 ) ;
#4444 = CYLINDRICAL_SURFACE ( 'NONE', #6652, 1.250000000000000444 ) ;
#4445 = ORIENTED_EDGE ( 'NONE', *, *, #6735, .F. ) ;
#4446 = EDGE_LOOP ( 'NONE', ( #291, #4897 ) ) ;
#4447 = CARTESIAN_POINT ( 'NONE',  ( 90.25000000000001421, 9.720002580593245511E-13, 0.000000000000000000 ) ) ;
#4448 = DIRECTION ( 'NONE',  ( -1.000000000000000000, 0.000000000000000000, 0.000000000000000000 ) ) ;
#4449 = PRESENTATION_STYLE_ASSIGNMENT (( #6786 ) ) ;
#4450 = VECTOR ( 'NONE', #1324, 1000.000000000000000 ) ;
#4451 = DIRECTION ( 'NONE',  ( -1.000000000000000000, 2.398081733190337496E-14, 0.000000000000000000 ) ) ;
#4452 = VERTEX_POINT ( 'NONE', #580 ) ;
#4453 = EDGE_LOOP ( 'NONE', ( #4211, #788, #3311, #5307 ) ) ;
#4454 = CIRCLE ( 'NONE', #1687, 5.249999999999976907 ) ;
#4455 = LINE ( 'NONE', #6351, #5166 ) ;
#4456 =( NAMED_UNIT ( * ) PLANE_ANGLE_UNIT ( ) SI_UNIT ( $, .RADIAN. ) );
#4457 = DIRECTION ( 'NONE',  ( -5.551115123125782702E-17, 0.000000000000000000, -1.000000000000000000 ) ) ;
#4458 = AXIS2_PLACEMENT_3D ( 'NONE', #7715, #4208, #66 ) ;
#4459 = CIRCLE ( 'NONE', #2464, 5.249999999999976907 ) ;
#4460 = CARTESIAN_POINT ( 'NONE',  ( -28.32536770618216693, 3.150165759062970583, 13.00000000000000178 ) ) ;
#4461 = ORIENTED_EDGE ( 'NONE', *, *, #1727, .F. ) ;
#4462 = EDGE_CURVE ( 'NONE', #5216, #194, #7165, .T. ) ;
#4463 = CIRCLE ( 'NONE', #3089, 4.999999999999990230 ) ;
#4464 = DIRECTION ( 'NONE',  ( 0.000000000000000000, 0.000000000000000000, 1.000000000000000000 ) ) ;
#4465 = FACE_OUTER_BOUND ( 'NONE', #2164, .T. ) ;
#4466 = CARTESIAN_POINT ( 'NONE',  ( -119.9981648402868046, 207.8429183184021554, 10.00000000000000000 ) ) ;
#4467 = CONTEXT_DEPENDENT_SHAPE_REPRESENTATION ( #2146, #6183 ) ;
#4468 = DIRECTION ( 'NONE',  ( -0.000000000000000000, 1.000000000000000000, 0.000000000000000000 ) ) ;
#4469 = EDGE_CURVE ( 'NONE', #2865, #4328, #7660, .T. ) ;
#4470 = AXIS2_PLACEMENT_3D ( 'NONE', #5264, #4000, #446 ) ;
#4471 = EDGE_LOOP ( 'NONE', ( #1881, #6947, #1291, #885 ) ) ;
#4472 = FACE_OUTER_BOUND ( 'NONE', #6893, .T. ) ;
#4473 = CARTESIAN_POINT ( 'NONE',  ( -68.76644452187068168, 49.96174644486002592, -40.00000000000000000 ) ) ;
#4474 = CLOSED_SHELL ( 'NONE', ( #3568, #2989, #5721, #5336, #1419, #862, #2560, #7542, #129, #6537, #6509, #3886, #229, #7282, #605, #7303, #2179, #5247, #471, #187, #1464, #521, #6836, #1144, #7744, #7172, #5092, #4416 ) ) ;
#4475 = DIRECTION ( 'NONE',  ( -0.1555099737793451675, 0.9878343221690302212, -1.110223024625155986E-18 ) ) ;
#4476 = CARTESIAN_POINT ( 'NONE',  ( -207.8429183184026670, 119.9981648402859378, -120.0000000000000000 ) ) ;
#4477 = DIRECTION ( 'NONE',  ( -0.5428387855420006014, 0.8398369204263920196, -2.550145071705742900E-17 ) ) ;
#4478 = PRODUCT_DEFINITION_SHAPE ( 'NONE', 'NONE',  #7776 ) ;
#4479 =( LENGTH_UNIT ( ) NAMED_UNIT ( * ) SI_UNIT ( .MILLI., .METRE. ) );
#4480 = ORIENTED_EDGE ( 'NONE', *, *, #411, .F. ) ;
#4481 = EDGE_LOOP ( 'NONE', ( #534, #7399, #5472, #5278 ) ) ;
#4482 = ORIENTED_EDGE ( 'NONE', *, *, #672, .F. ) ;
#4483 = ADVANCED_FACE ( 'NONE', ( #652, #3654, #1847, #3066, #5465, #62, #7283 ), #1164, .T. ) ;
#4484 = VERTEX_POINT ( 'NONE', #691 ) ;
#4485 = CIRCLE ( 'NONE', #4495, 37.49999999999997868 ) ;
#4486 = LINE ( 'NONE', #3345, #4671 ) ;
#4487 = LINE ( 'NONE', #7481, #6049 ) ;
#4488 =( LENGTH_UNIT ( ) NAMED_UNIT ( * ) SI_UNIT ( .MILLI., .METRE. ) );
#4489 = CARTESIAN_POINT ( 'NONE',  ( 202.5929183184021269, 119.9981648402868331, -8.673617379884035472E-15 ) ) ;
#4490 = VERTEX_POINT ( 'NONE', #7325 ) ;
#4491 = ORIENTED_EDGE ( 'NONE', *, *, #6873, .F. ) ;
#4492 = PRODUCT_DEFINITION_CONTEXT ( 'detailed design', #6770, 'design' ) ;
#4493 = ORIENTED_EDGE ( 'NONE', *, *, #3841, .F. ) ;
#4494 = FACE_OUTER_BOUND ( 'NONE', #6042, .T. ) ;
#4495 = AXIS2_PLACEMENT_3D ( 'NONE', #6436, #2891, #7103 ) ;
#4496 = DIRECTION ( 'NONE',  ( -0.000000000000000000, -0.000000000000000000, 1.000000000000000000 ) ) ;
#4497 = CARTESIAN_POINT ( 'NONE',  ( -2.081668171172168513E-14, -9.237604307034017026, -0.7145311798163319628 ) ) ;
#4498 = EDGE_LOOP ( 'NONE', ( #7102, #7466, #7148, #6110 ) ) ;
#4499 = VECTOR ( 'NONE', #5063, 1000.000000000000000 ) ;
#4500 = PRODUCT_RELATED_PRODUCT_CATEGORY ( 'part', '', ( #1453 ) ) ;
#4501 = CARTESIAN_POINT ( 'NONE',  ( 0.000000000000000000, 0.000000000000000000, 576.0908266162076643 ) ) ;
#4502 = CARTESIAN_POINT ( 'NONE',  ( 0.000000000000000000, -150.0000000000000568, 0.000000000000000000 ) ) ;
#4503 = CARTESIAN_POINT ( 'NONE',  ( 28.05900627794855851, 4.994213320838720271, -79.99999999999995737 ) ) ;
#4504 = VECTOR ( 'NONE', #136, 1000.000000000000000 ) ;
#4505 = DIRECTION ( 'NONE',  ( 0.000000000000000000, 0.000000000000000000, 1.000000000000000000 ) ) ;
#4506 = EDGE_LOOP ( 'NONE', ( #1149, #3651, #4544, #1403 ) ) ;
#4507 = EDGE_CURVE ( 'NONE', #926, #4597, #3890, .T. ) ;
#4508 = DIRECTION ( 'NONE',  ( -0.000000000000000000, -0.000000000000000000, 1.000000000000000000 ) ) ;
#4509 = AXIS2_PLACEMENT_3D ( 'NONE', #7462, #5764, #276 ) ;
#4510 = DIRECTION ( 'NONE',  ( 1.000000000000000000, 0.000000000000000000, 0.000000000000000000 ) ) ;
#4511 = EDGE_CURVE ( 'NONE', #7759, #3431, #5987, .T. ) ;
#4512 = EDGE_CURVE ( 'NONE', #7398, #6870, #3637, .T. ) ;
#4513 = DIRECTION ( 'NONE',  ( -0.000000000000000000, -0.000000000000000000, 1.000000000000000000 ) ) ;
#4514 = CARTESIAN_POINT ( 'NONE',  ( 26.26644452187122170, -80.83980388508783221, 10.00000000000000000 ) ) ;
#4515 = DIRECTION ( 'NONE',  ( -1.000000000000000000, 4.286207611454020849E-16, 0.000000000000000000 ) ) ;
#4516 = CIRCLE ( 'NONE', #2889, 5.249999999999988454 ) ;
#4517 = EDGE_CURVE ( 'NONE', #1930, #1025, #2517, .T. ) ;
#4518 = CYLINDRICAL_SURFACE ( 'NONE', #1437, 5.249999999999976907 ) ;
#4519 = ORIENTED_EDGE ( 'NONE', *, *, #7657, .T. ) ;
#4520 = ORIENTED_EDGE ( 'NONE', *, *, #7691, .F. ) ;
#4521 = ORIENTED_EDGE ( 'NONE', *, *, #3747, .F. ) ;
#4522 = CIRCLE ( 'NONE', #5139, 30.00000000000000000 ) ;
#4523 = EDGE_CURVE ( 'NONE', #6148, #7619, #4163, .T. ) ;
#4524 = CARTESIAN_POINT ( 'NONE',  ( 2.750000000000000000, -33.63777638310832430, 0.000000000000000000 ) ) ;
#4525 = LINE ( 'NONE', #6934, #6163 ) ;
#4526 = CARTESIAN_POINT ( 'NONE',  ( 89.90381056766652534, -74.99999999999882050, 10.00000000000000000 ) ) ;
#4527 = SURFACE_STYLE_FILL_AREA ( #5555 ) ;
#4528 = CARTESIAN_POINT ( 'NONE',  ( 32.49999999999997158, 3.980102097228894682E-15, -93.00430309513780003 ) ) ;
#4529 = EDGE_CURVE ( 'NONE', #1972, #1601, #7166, .T. ) ;
#4530 = CONICAL_SURFACE ( 'NONE', #3154, 4.999999999999990230, 0.7853981633974524978 ) ;
#4531 = VERTEX_POINT ( 'NONE', #6618 ) ;
#4532 = VERTEX_POINT ( 'NONE', #3731 ) ;
#4533 = ORIENTED_EDGE ( 'NONE', *, *, #2539, .F. ) ;
#4534 = DIRECTION ( 'NONE',  ( 0.000000000000000000, 0.000000000000000000, 1.000000000000000000 ) ) ;
#4535 = DIRECTION ( 'NONE',  ( 1.000000000000000000, 0.000000000000000000, 0.000000000000000000 ) ) ;
#4536 = DIRECTION ( 'NONE',  ( -0.000000000000000000, -0.000000000000000000, -1.000000000000000000 ) ) ;
#4537 = ORIENTED_EDGE ( 'NONE', *, *, #5388, .T. ) ;
#4538 = CIRCLE ( 'NONE', #1511, 29.99999999999999289 ) ;
#4539 = CARTESIAN_POINT ( 'NONE',  ( 207.8429183184020985, 119.9981648402868331, -8.673617379884035472E-15 ) ) ;
#4540 = PLANE ( 'NONE',  #6355 ) ;
#4541 = VECTOR ( 'NONE', #739, 1000.000000000000000 ) ;
#4542 = CARTESIAN_POINT ( 'NONE',  ( -63.76644452187068879, 49.96174644486002592, 24.17200000000001125 ) ) ;
#4543 = DIRECTION ( 'NONE',  ( 0.000000000000000000, 0.000000000000000000, -1.000000000000000000 ) ) ;
#4544 = ORIENTED_EDGE ( 'NONE', *, *, #3842, .F. ) ;
#4545 = DIRECTION ( 'NONE',  ( 1.000000000000000000, 0.000000000000000000, 0.000000000000000000 ) ) ;
#4546 = CARTESIAN_POINT ( 'NONE',  ( -4.000000000000004441, 6.928203230275506108, -4.700000000000000178 ) ) ;
#4547 = FACE_OUTER_BOUND ( 'NONE', #6035, .T. ) ;
#4548 = FACE_OUTER_BOUND ( 'NONE', #1693, .T. ) ;
#4549 = CARTESIAN_POINT ( 'NONE',  ( 0.000000000000000000, 0.000000000000000000, 0.000000000000000000 ) ) ;
#4550 = ITEM_DEFINED_TRANSFORMATION ( 'NONE', 'NONE', #6995,  #7485 ) ;
#4551 = CARTESIAN_POINT ( 'NONE',  ( 119.9981648402866341, 207.8429183184022122, -50.00000000000000000 ) ) ;
#4552 = EDGE_CURVE ( 'NONE', #5239, #5661, #1205, .T. ) ;
#4553 = ORIENTED_EDGE ( 'NONE', *, *, #1184, .F. ) ;
#4554 = ORIENTED_EDGE ( 'NONE', *, *, #7187, .T. ) ;
#4555 = ADVANCED_FACE ( 'NONE', ( #618 ), #3031, .F. ) ;
#4556 = B_SPLINE_CURVE_WITH_KNOTS ( 'NONE', 3,
 ( #591, #6586, #1176, #2881, #3547, #7717 ),
 .UNSPECIFIED., .F., .F.,
 ( 4, 2, 4 ),
 ( 0.008240550023493525833, 0.01057684187039405199, 0.01291313371729457642 ),
 .UNSPECIFIED. ) ;
#4557 = ORIENTED_EDGE ( 'NONE', *, *, #2651, .T. ) ;
#4558 = VECTOR ( 'NONE', #4468, 1000.000000000000000 ) ;
#4559 = EDGE_CURVE ( 'NONE', #2491, #5454, #5429, .T. ) ;
#4560 = LINE ( 'NONE', #6968, #4599 ) ;
#4561 = DIRECTION ( 'NONE',  ( 1.000000000000000000, 0.000000000000000000, 0.000000000000000000 ) ) ;
#4562 = CARTESIAN_POINT ( 'NONE',  ( -3.500000000000006661, 0.000000000000000000, 0.000000000000000000 ) ) ;
#4563 = CARTESIAN_POINT ( 'NONE',  ( -8.000000000000000000, 3.871967595402119766, -0.4989386132324563627 ) ) ;
#4564 = FILL_AREA_STYLE_COLOUR ( '', #3592 ) ;
#4565 = FACE_OUTER_BOUND ( 'NONE', #6059, .T. ) ;
#4566 = CIRCLE ( 'NONE', #665, 150.0000000000000568 ) ;
#4567 = FACE_OUTER_BOUND ( 'NONE', #5780, .T. ) ;
#4568 = EDGE_CURVE ( 'NONE', #816, #4169, #1963, .T. ) ;
#4569 = EDGE_LOOP ( 'NONE', ( #6489, #7562, #2947, #6301 ) ) ;
#4570 = ORIENTED_EDGE ( 'NONE', *, *, #4412, .F. ) ;
#4571 = EDGE_LOOP ( 'NONE', ( #4131, #2375 ) ) ;
#4572 = AXIS2_PLACEMENT_3D ( 'NONE', #7330, #1701, #29 ) ;
#4573 = CARTESIAN_POINT ( 'NONE',  ( 207.8429183184020985, 119.9981648402868331, -8.673617379884035472E-15 ) ) ;
#4574 = DIRECTION ( 'NONE',  ( 0.000000000000000000, 0.000000000000000000, -1.000000000000000000 ) ) ;
#4575 = CARTESIAN_POINT ( 'NONE',  ( 2.645508037661878475, 7.710219529346607814, -0.06809871960542819569 ) ) ;
#4576 = AXIS2_PLACEMENT_3D ( 'NONE', #4295, #7298, #3707 ) ;
#4577 = ORIENTED_EDGE ( 'NONE', *, *, #6397, .F. ) ;
#4578 = FACE_OUTER_BOUND ( 'NONE', #2575, .T. ) ;
#4579 = DIRECTION ( 'NONE',  ( 0.000000000000000000, 0.000000000000000000, -1.000000000000000000 ) ) ;
#4580 = AXIS2_PLACEMENT_3D ( 'NONE', #3864, #857, #1491 ) ;
#4581 = CARTESIAN_POINT ( 'NONE',  ( 37.49999999999997868, 4.592425496802572000E-15, -119.9999999999999858 ) ) ;
#4582 = LINE ( 'NONE', #3481, #4687 ) ;
#4583 = ORIENTED_EDGE ( 'NONE', *, *, #3403, .F. ) ;
#4584 = AXIS2_PLACEMENT_3D ( 'NONE', #3900, #3307, #301 ) ;
#4585 =( GEOMETRIC_REPRESENTATION_CONTEXT ( 3 ) GLOBAL_UNCERTAINTY_ASSIGNED_CONTEXT ( ( #4376 ) ) GLOBAL_UNIT_ASSIGNED_CONTEXT ( ( #2343, #4135, #5955 ) ) REPRESENTATION_CONTEXT ( 'NONE', 'WORKASPACE' ) );
#4586 = CARTESIAN_POINT ( 'NONE',  ( -73.76644452187066747, 49.96174644486002592, 24.17200000000001125 ) ) ;
#4587 = PRESENTATION_STYLE_ASSIGNMENT (( #365 ) ) ;
#4588 = CARTESIAN_POINT ( 'NONE',  ( 0.000000000000000000, 0.000000000000000000, -139.9999999999999716 ) ) ;
#4589 = DIRECTION ( 'NONE',  ( -0.000000000000000000, -0.000000000000000000, 1.000000000000000000 ) ) ;
#4590 = CARTESIAN_POINT ( 'NONE',  ( 0.000000000000000000, 5.857142857142855874, 3.859999999999999876 ) ) ;
#4591 = CONTEXT_DEPENDENT_SHAPE_REPRESENTATION ( #627, #3034 ) ;
#4592 = CIRCLE ( 'NONE', #6109, 28.50000000000000355 ) ;
#4593 = LINE ( 'NONE', #3449, #4340 ) ;
#4594 = VERTEX_POINT ( 'NONE', #5105 ) ;
#4595 = APPLICATION_CONTEXT ( 'automotive_design' ) ;
#4596 = ORIENTED_EDGE ( 'NONE', *, *, #3309, .F. ) ;
#4597 = VERTEX_POINT ( 'NONE', #3921 ) ;
#4598 = AXIS2_PLACEMENT_3D ( 'NONE', #7753, #3068, #2372 ) ;
#4599 = VECTOR ( 'NONE', #1562, 1000.000000000000000 ) ;
#4600 = ADVANCED_FACE ( 'NONE', ( #6886 ), #7505, .F. ) ;
#4601 = CARTESIAN_POINT ( 'NONE',  ( -7.345652830558756285, 4.996589667937373136, -4.203584543331207790 ) ) ;
#4602 = DIRECTION ( 'NONE',  ( -1.000000000000000000, 0.000000000000000000, 0.000000000000000000 ) ) ;
#4603 = CARTESIAN_POINT ( 'NONE',  ( -68.76644452187068168, 49.96174644486002592, 0.000000000000000000 ) ) ;
#4604 = CYLINDRICAL_SURFACE ( 'NONE', #6809, 10.00000000000000178 ) ;
#4605 = DIRECTION ( 'NONE',  ( 0.000000000000000000, 0.000000000000000000, 1.000000000000000000 ) ) ;
#4606 =( NAMED_UNIT ( * ) SI_UNIT ( $, .STERADIAN. ) SOLID_ANGLE_UNIT ( ) );
#4607 = FACE_OUTER_BOUND ( 'NONE', #6075, .T. ) ;
#4608 = EDGE_CURVE ( 'NONE', #587, #6167, #353, .T. ) ;
#4609 = ORIENTED_EDGE ( 'NONE', *, *, #6407, .T. ) ;
#4610 = ORIENTED_EDGE ( 'NONE', *, *, #5473, .T. ) ;
#4611 = ORIENTED_EDGE ( 'NONE', *, *, #7040, .F. ) ;
#4612 = CYLINDRICAL_SURFACE ( 'NONE', #5552, 5.249999999999997335 ) ;
#4613 = EDGE_CURVE ( 'NONE', #7150, #699, #5585, .T. ) ;
#4614 =( LENGTH_UNIT ( ) NAMED_UNIT ( * ) SI_UNIT ( .MILLI., .METRE. ) );
#4615 = LINE ( 'NONE', #4688, #7726 ) ;
#4616 = AXIS2_PLACEMENT_3D ( 'NONE', #132, #7196, #4902 ) ;
#4617 = ADVANCED_FACE ( 'NONE', ( #6180 ), #6293, .F. ) ;
#4618 = CARTESIAN_POINT ( 'NONE',  ( 0.000000000000000000, 0.000000000000000000, 0.000000000000000000 ) ) ;
#4619 = ORIENTED_EDGE ( 'NONE', *, *, #3670, .F. ) ;
#4620 = EDGE_CURVE ( 'NONE', #380, #2748, #1111, .T. ) ;
#4621 = DIRECTION ( 'NONE',  ( -1.000000000000000000, 1.224646799147352961E-16, 0.000000000000000000 ) ) ;
#4622 = FACE_OUTER_BOUND ( 'NONE', #5873, .T. ) ;
#4623 = CARTESIAN_POINT ( 'NONE',  ( -68.76644452187068168, 49.96174644486002592, 24.17200000000001125 ) ) ;
#4624 = FACE_OUTER_BOUND ( 'NONE', #5149, .T. ) ;
#4625 = EDGE_CURVE ( 'NONE', #5872, #5391, #3383, .T. ) ;
#4626 = VERTEX_POINT ( 'NONE', #7395 ) ;
#4627 = ORIENTED_EDGE ( 'NONE', *, *, #2461, .F. ) ;
#4628 = DIRECTION ( 'NONE',  ( 1.000000000000000000, 0.000000000000000000, 0.000000000000000000 ) ) ;
#4629 =( NAMED_UNIT ( * ) SI_UNIT ( $, .STERADIAN. ) SOLID_ANGLE_UNIT ( ) );
#4630 = DIRECTION ( 'NONE',  ( 1.000000000000000000, 0.000000000000000000, 0.000000000000000000 ) ) ;
#4631 = DIRECTION ( 'NONE',  ( 1.000000000000000000, 0.000000000000000000, 0.000000000000000000 ) ) ;
#4632 = DIRECTION ( 'NONE',  ( 1.000000000000000000, 0.000000000000000000, 0.000000000000000000 ) ) ;
#4633 = ITEM_DEFINED_TRANSFORMATION ( 'NONE', 'NONE', #5993,  #7485 ) ;
#4634 = CARTESIAN_POINT ( 'NONE',  ( -68.76644452187068168, 49.96174644486002592, -40.00000000000000000 ) ) ;
#4635 = ORIENTED_EDGE ( 'NONE', *, *, #4896, .T. ) ;
#4636 = ORIENTED_EDGE ( 'NONE', *, *, #4228, .T. ) ;
#4637 = CIRCLE ( 'NONE', #6153, 35.00000000000000711 ) ;
#4638 = VERTEX_POINT ( 'NONE', #879 ) ;
#4639 = CARTESIAN_POINT ( 'NONE',  ( 8.000000000000000000, 4.618802153517013842, -3.985468820183668104 ) ) ;
#4640 = AXIS2_PLACEMENT_3D ( 'NONE', #1644, #1087, #7674 ) ;
#4641 = FACE_OUTER_BOUND ( 'NONE', #473, .T. ) ;
#4642 = CARTESIAN_POINT ( 'NONE',  ( 28.32536770618216693, -3.150165759062972359, 13.00000000000000178 ) ) ;
#4643 = CARTESIAN_POINT ( 'NONE',  ( 0.000000000000000000, 0.000000000000000000, 0.000000000000000000 ) ) ;
#4644 = FILL_AREA_STYLE ('',( #2335 ) ) ;
#4645 = CYLINDRICAL_SURFACE ( 'NONE', #2008, 5.249999999999976907 ) ;
#4646 = ORIENTED_EDGE ( 'NONE', *, *, #4179, .F. ) ;
#4647 = CIRCLE ( 'NONE', #3772, 40.00000000000000711 ) ;
#4648 = VERTEX_POINT ( 'NONE', #2002 ) ;
#4649 = ORIENTED_EDGE ( 'NONE', *, *, #4995, .F. ) ;
#4650 = CARTESIAN_POINT ( 'NONE',  ( -5.554394503829287011, 27.95350964898380752, -79.99999999999995737 ) ) ;
#4651 = LINE ( 'NONE', #3473, #2955 ) ;
#4652 = FACE_OUTER_BOUND ( 'NONE', #7428, .T. ) ;
#4653 = EDGE_CURVE ( 'NONE', #4093, #2529, #919, .T. ) ;
#4654 = ORIENTED_EDGE ( 'NONE', *, *, #5823, .F. ) ;
#4655 = EDGE_CURVE ( 'NONE', #1789, #4093, #5163, .T. ) ;
#4656 = ADVANCED_FACE ( 'NONE', ( #804 ), #3295, .T. ) ;
#4657 = ADVANCED_FACE ( 'NONE', ( #6811 ), #2082, .F. ) ;
#4658 = CARTESIAN_POINT ( 'NONE',  ( 0.000000000000000000, 0.000000000000000000, 0.000000000000000000 ) ) ;
#4659 = CARTESIAN_POINT ( 'NONE',  ( -58.76644452187068168, 49.96174644486002592, 0.000000000000000000 ) ) ;
#4660 = CARTESIAN_POINT ( 'NONE',  ( -199.9963296805737230, 0.000000000000000000, 0.000000000000000000 ) ) ;
#4661 = AXIS2_PLACEMENT_3D ( 'NONE', #7379, #1986, #6196 ) ;
#4662 = CARTESIAN_POINT ( 'NONE',  ( 39.64284999284935651, 144.6666666666667140, 0.000000000000000000 ) ) ;
#4663 = EDGE_LOOP ( 'NONE', ( #7032, #3238, #6513, #5899 ) ) ;
#4664 = EDGE_LOOP ( 'NONE', ( #5740, #3074, #3508 ) ) ;
#4665 = CARTESIAN_POINT ( 'NONE',  ( 0.000000000000000000, 0.000000000000000000, -93.00430309513780003 ) ) ;
#4666 = DIRECTION ( 'NONE',  ( 0.000000000000000000, 0.000000000000000000, 1.000000000000000000 ) ) ;
#4667 = CARTESIAN_POINT ( 'NONE',  ( 0.000000000000000000, 0.000000000000000000, 0.000000000000000000 ) ) ;
#4668 = DIRECTION ( 'NONE',  ( 0.000000000000000000, 0.000000000000000000, 1.000000000000000000 ) ) ;
#4669 = CONTEXT_DEPENDENT_SHAPE_REPRESENTATION ( #516, #6678 ) ;
#4670 = DIRECTION ( 'NONE',  ( 0.000000000000000000, 0.000000000000000000, -1.000000000000000000 ) ) ;
#4671 = VECTOR ( 'NONE', #4405, 1000.000000000000000 ) ;
#4672 = ORIENTED_EDGE ( 'NONE', *, *, #1027, .F. ) ;
#4673 = ORIENTED_EDGE ( 'NONE', *, *, #1731, .T. ) ;
#4674 = VERTEX_POINT ( 'NONE', #5028 ) ;
#4675 = CARTESIAN_POINT ( 'NONE',  ( 199.9963296805737230, -4.796075449120964792E-12, -82.99999999999998579 ) ) ;
#4676 = CARTESIAN_POINT ( 'NONE',  ( -8.000000000000000000, -4.618802153517012954, -4.700000000000000178 ) ) ;
#4677 = CARTESIAN_POINT ( 'NONE',  ( 0.000000000000000000, 0.000000000000000000, -119.9999999999999858 ) ) ;
#4678 = CARTESIAN_POINT ( 'NONE',  ( -68.76644452187028378, -49.96174644486062277, 14.69999999999999929 ) ) ;
#4679 = CARTESIAN_POINT ( 'NONE',  ( -68.76644452187068168, 49.96174644486002592, -64.17200000000001125 ) ) ;
#4680 = DIRECTION ( 'NONE',  ( 0.000000000000000000, -0.000000000000000000, -1.000000000000000000 ) ) ;
#4681 = ORIENTED_EDGE ( 'NONE', *, *, #125, .T. ) ;
#4682 = ORIENTED_EDGE ( 'NONE', *, *, #6065, .T. ) ;
#4683 = EDGE_LOOP ( 'NONE', ( #4105, #1418 ) ) ;
#4684 = DIRECTION ( 'NONE',  ( -3.081487911019577365E-33, 2.775557561562891967E-17, 1.000000000000000000 ) ) ;
#4685 = DIRECTION ( 'NONE',  ( 1.000000000000000000, 0.000000000000000000, 0.000000000000000000 ) ) ;
#4686 = SHAPE_REPRESENTATION_RELATIONSHIP ( 'NONE' , 'NONE' ,  #2561, #5011 ) ;
#4687 = VECTOR ( 'NONE', #7031, 1000.000000000000000 ) ;
#4688 = CARTESIAN_POINT ( 'NONE',  ( -4.681546503268407275E-16, 9.237604307034017026, -4.700000000000000178 ) ) ;
#4689 = CARTESIAN_POINT ( 'NONE',  ( 119.9981648402866341, 207.8429183184022122, -50.00000000000000000 ) ) ;
#4690 = ORIENTED_EDGE ( 'NONE', *, *, #1278, .F. ) ;
#4691 = EDGE_LOOP ( 'NONE', ( #1442, #3002, #2663, #2864 ) ) ;
#4692 = AXIS2_PLACEMENT_3D ( 'NONE', #3171, #3872, #4342 ) ;
#4693 = CARTESIAN_POINT ( 'NONE',  ( -2.750000000000000000, -33.63777638310832430, -3.000000000000000000 ) ) ;
#4694 = CARTESIAN_POINT ( 'NONE',  ( 0.000000000000000000, 0.000000000000000000, 0.000000000000000000 ) ) ;
#4695 =( REPRESENTATION_RELATIONSHIP ('NONE','NONE', #1229, #1433 ) REPRESENTATION_RELATIONSHIP_WITH_TRANSFORMATION ( #1037 )SHAPE_REPRESENTATION_RELATIONSHIP( ) );
#4696 = DIRECTION ( 'NONE',  ( 0.000000000000000000, 0.000000000000000000, 1.000000000000000000 ) ) ;
#4697 = AXIS2_PLACEMENT_3D ( 'NONE', #3697, #6660, #3071 ) ;
#4698 = CARTESIAN_POINT ( 'NONE',  ( -5.690023276062397883, -5.952467836904158816, -4.569346954796184690 ) ) ;
#4699 = ORIENTED_EDGE ( 'NONE', *, *, #3028, .F. ) ;
#4700 = EDGE_CURVE ( 'NONE', #1609, #1582, #4516, .T. ) ;
#4701 = ORIENTED_EDGE ( 'NONE', *, *, #314, .T. ) ;
#4702 = DIRECTION ( 'NONE',  ( -0.000000000000000000, -0.000000000000000000, 1.000000000000000000 ) ) ;
#4703 = AXIS2_PLACEMENT_3D ( 'NONE', #976, #6393, #4535 ) ;
#4704 = B_SPLINE_CURVE_WITH_KNOTS ( 'NONE', 3,
 ( #1565, #6971, #537, #5270, #1732, #3537 ),
 .UNSPECIFIED., .F., .F.,
 ( 4, 2, 4 ),
 ( 0.008240550023493527568, 0.01057684187039405199, 0.01291313371729457642 ),
 .UNSPECIFIED. ) ;
#4705 = CARTESIAN_POINT ( 'NONE',  ( -5.459126460941067016, -34.89491303563345070, -3.000000000000000000 ) ) ;
#4706 = DIRECTION ( 'NONE',  ( 1.000000000000000000, 0.000000000000000000, 0.000000000000000000 ) ) ;
#4707 = CYLINDRICAL_SURFACE ( 'NONE', #970, 199.9963296805737230 ) ;
#4708 = ADVANCED_FACE ( 'NONE', ( #1434 ), #6254, .F. ) ;
#4709 = DIRECTION ( 'NONE',  ( 1.000000000000000000, 0.000000000000000000, 0.000000000000000000 ) ) ;
#4710 = PRODUCT_DEFINITION_CONTEXT ( 'detailed design', #7516, 'design' ) ;
#4711 = VECTOR ( 'NONE', #4451, 1000.000000000000000 ) ;
#4712 = VERTEX_POINT ( 'NONE', #2667 ) ;
#4713 = CIRCLE ( 'NONE', #2202, 35.97500000000000853 ) ;
#4714 = ORIENTED_EDGE ( 'NONE', *, *, #4418, .T. ) ;
#4715 = ORIENTED_EDGE ( 'NONE', *, *, #2792, .F. ) ;
#4716 = FACE_OUTER_BOUND ( 'NONE', #4810, .T. ) ;
#4717 = CIRCLE ( 'NONE', #1828, 30.00000000000000000 ) ;
#4718 = CARTESIAN_POINT ( 'NONE',  ( 3.499999999999996003, 0.000000000000000000, 0.000000000000000000 ) ) ;
#4719 = CYLINDRICAL_SURFACE ( 'NONE', #5887, 37.50000000000000000 ) ;
#4720 = CARTESIAN_POINT ( 'NONE',  ( 0.000000000000000000, 0.000000000000000000, -50.00000000000000000 ) ) ;
#4721 = DIRECTION ( 'NONE',  ( 1.000000000000000000, 0.000000000000000000, 0.000000000000000000 ) ) ;
#4722 = CARTESIAN_POINT ( 'NONE',  ( 0.000000000000000000, 0.000000000000000000, -3.000000000000000000 ) ) ;
#4723 = EDGE_CURVE ( 'NONE', #47, #7320, #5062, .T. ) ;
#4724 = VERTEX_POINT ( 'NONE', #4035 ) ;
#4725 =( GEOMETRIC_REPRESENTATION_CONTEXT ( 3 ) GLOBAL_UNCERTAINTY_ASSIGNED_CONTEXT ( ( #826 ) ) GLOBAL_UNIT_ASSIGNED_CONTEXT ( ( #6861, #6192, #2643 ) ) REPRESENTATION_CONTEXT ( 'NONE', 'WORKASPACE' ) );
#4726 = ORIENTED_EDGE ( 'NONE', *, *, #662, .T. ) ;
#4727 = ORIENTED_EDGE ( 'NONE', *, *, #6970, .T. ) ;
#4728 = DIRECTION ( 'NONE',  ( 0.000000000000000000, 0.000000000000000000, 1.000000000000000000 ) ) ;
#4729 = CARTESIAN_POINT ( 'NONE',  ( -32.49999999999997158, 0.000000000000000000, -109.9956969048621716 ) ) ;
#4730 = DIRECTION ( 'NONE',  ( 0.000000000000000000, -1.000000000000000000, 0.000000000000000000 ) ) ;
#4731 = CIRCLE ( 'NONE', #3852, 5.250000000000004441 ) ;
#4732 = VERTEX_POINT ( 'NONE', #3374 ) ;
#4733 = CIRCLE ( 'NONE', #4353, 5.249999999999991118 ) ;
#4734 = CARTESIAN_POINT ( 'NONE',  ( -10.00000000000000000, 41.99999999999999289, -60.00000000000000711 ) ) ;
#4735 = DIRECTION ( 'NONE',  ( -0.000000000000000000, -0.000000000000000000, 1.000000000000000000 ) ) ;
#4736 = AXIS2_PLACEMENT_3D ( 'NONE', #3286, #2070, #1993 ) ;
#4737 = CARTESIAN_POINT ( 'NONE',  ( 0.000000000000000000, 0.000000000000000000, -60.00000000000000711 ) ) ;
#4738 = DIRECTION ( 'NONE',  ( 1.000000000000000000, 0.000000000000000000, 0.000000000000000000 ) ) ;
#4739 = EDGE_LOOP ( 'NONE', ( #1371, #6429, #5250, #4461 ) ) ;
#4740 = PRODUCT_RELATED_PRODUCT_CATEGORY ( 'part', '', ( #5672 ) ) ;
#4741 = VERTEX_POINT ( 'NONE', #5852 ) ;
#4742 = AXIS2_PLACEMENT_3D ( 'NONE', #5840, #6990, #3987 ) ;
#4743 = EDGE_LOOP ( 'NONE', ( #586, #7748 ) ) ;
#4744 = FILL_AREA_STYLE ('',( #6997 ) ) ;
#4745 = DIRECTION ( 'NONE',  ( 1.000000000000000000, 0.000000000000000000, 0.000000000000000000 ) ) ;
#4746 = LINE ( 'NONE', #6015, #743 ) ;
#4747 = DIRECTION ( 'NONE',  ( 5.551115123125782702E-17, -0.000000000000000000, 1.000000000000000000 ) ) ;
#4748 = CONTEXT_DEPENDENT_SHAPE_REPRESENTATION ( #4144, #7183 ) ;
#4749 = AXIS2_PLACEMENT_3D ( 'NONE', #6498, #2995, #3578 ) ;
#4750 = DIRECTION ( 'NONE',  ( -1.000000000000000000, 0.000000000000000000, 0.000000000000000000 ) ) ;
#4751 = ORIENTED_EDGE ( 'NONE', *, *, #5439, .T. ) ;
#4752 = EDGE_CURVE ( 'NONE', #256, #1043, #2277, .T. ) ;
#4753 = ORIENTED_EDGE ( 'NONE', *, *, #82, .T. ) ;
#4754 = ADVANCED_FACE ( 'NONE', ( #5178 ), #2322, .F. ) ;
#4755 = EDGE_CURVE ( 'NONE', #6520, #257, #329, .T. ) ;
#4756 = VECTOR ( 'NONE', #3646, 1000.000000000000000 ) ;
#4757 = DIRECTION ( 'NONE',  ( 1.000000000000000000, 0.000000000000000000, 0.000000000000000000 ) ) ;
#4758 = EDGE_CURVE ( 'NONE', #1496, #147, #5276, .T. ) ;
#4759 = CARTESIAN_POINT ( 'NONE',  ( -125.2481648402867762, 207.8429183184021554, 10.00000000000000000 ) ) ;
#4760 = CARTESIAN_POINT ( 'NONE',  ( -1.728922298134113098E-15, 8.513302795252935035E-16, 13.00000000000000178 ) ) ;
#4761 = CARTESIAN_POINT ( 'NONE',  ( 4.793225973945551641E-15, 0.000000000000000000, -116.4999999999999716 ) ) ;
#4762 = DIRECTION ( 'NONE',  ( 1.000000000000000000, 0.000000000000000000, 0.000000000000000000 ) ) ;
#4763 = LINE ( 'NONE', #3036, #1770 ) ;
#4764 = ORIENTED_EDGE ( 'NONE', *, *, #895, .T. ) ;
#4765 = ADVANCED_FACE ( 'NONE', ( #4548 ), #2820, .F. ) ;
#4766 = ORIENTED_EDGE ( 'NONE', *, *, #223, .F. ) ;
#4767 = ORIENTED_EDGE ( 'NONE', *, *, #1178, .F. ) ;
#4768 = VECTOR ( 'NONE', #5642, 1000.000000000000000 ) ;
#4769 = DIRECTION ( 'NONE',  ( 0.5000000000000101030, -0.8660254037844328234, 0.000000000000000000 ) ) ;
#4770 = FILL_AREA_STYLE ('',( #1058 ) ) ;
#4771 =( LENGTH_UNIT ( ) NAMED_UNIT ( * ) SI_UNIT ( .MILLI., .METRE. ) );
#4772 = CARTESIAN_POINT ( 'NONE',  ( 114.7481648402869041, 207.8429183184021269, 10.00000000000000178 ) ) ;
#4773 = ORIENTED_EDGE ( 'NONE', *, *, #32, .F. ) ;
#4774 = ORIENTED_EDGE ( 'NONE', *, *, #5086, .T. ) ;
#4775 = CIRCLE ( 'NONE', #3146, 1.250000000000000222 ) ;
#4776 = DIRECTION ( 'NONE',  ( 0.000000000000000000, 0.000000000000000000, 1.000000000000000000 ) ) ;
#4777 = CARTESIAN_POINT ( 'NONE',  ( 37.49999999999997868, 4.592425496802572000E-15, -112.9999999999999716 ) ) ;
#4778 = CARTESIAN_POINT ( 'NONE',  ( -68.76644452187068168, 49.96174644486002592, -40.00000000000000000 ) ) ;
#4779 = ORIENTED_EDGE ( 'NONE', *, *, #2680, .F. ) ;
#4780 = VECTOR ( 'NONE', #3463, 1000.000000000000000 ) ;
#4781 = ORIENTED_EDGE ( 'NONE', *, *, #1668, .T. ) ;
#4782 = ORIENTED_EDGE ( 'NONE', *, *, #7584, .T. ) ;
#4783 = PRODUCT_DEFINITION_SHAPE ( 'NONE', 'NONE',  #7769 ) ;
#4784 = CARTESIAN_POINT ( 'NONE',  ( 79.75000000000000000, 9.726431976288768917E-13, 0.000000000000000000 ) ) ;
#4785 = CARTESIAN_POINT ( 'NONE',  ( 29.99999999999999289, 0.000000000000000000, 10.00000000000000888 ) ) ;
#4786 = LINE ( 'NONE', #5423, #5783 ) ;
#4787 = DIRECTION ( 'NONE',  ( 0.000000000000000000, 0.000000000000000000, 1.000000000000000000 ) ) ;
#4788 = UNCERTAINTY_MEASURE_WITH_UNIT (LENGTH_MEASURE( 1.000000000000000082E-05 ), #5810, 'distance_accuracy_value', 'NONE');
#4789 = DIRECTION ( 'NONE',  ( 1.000000000000000000, 0.000000000000000000, 0.000000000000000000 ) ) ;
#4790 = ORIENTED_EDGE ( 'NONE', *, *, #6735, .T. ) ;
#4791 = ORIENTED_EDGE ( 'NONE', *, *, #2159, .F. ) ;
#4792 = AXIS2_PLACEMENT_3D ( 'NONE', #4338, #6756, #160 ) ;
#4793 = DIRECTION ( 'NONE',  ( -1.000000000000000000, 2.403401228516536636E-14, 0.000000000000000000 ) ) ;
#4794 = ADVANCED_FACE ( 'NONE', ( #7581 ), #6960, .T. ) ;
#4795 = DIRECTION ( 'NONE',  ( 1.000000000000000000, 0.000000000000000000, 0.000000000000000000 ) ) ;
#4796 = DIRECTION ( 'NONE',  ( 1.000000000000000000, 0.000000000000000000, 0.000000000000000000 ) ) ;
#4797 = CARTESIAN_POINT ( 'NONE',  ( 0.000000000000000000, 0.000000000000000000, 0.000000000000000000 ) ) ;
#4798 = AXIS2_PLACEMENT_3D ( 'NONE', #1292, #1215, #590 ) ;
#4799 = SURFACE_SIDE_STYLE ('',( #1322 ) ) ;
#4800 = CYLINDRICAL_SURFACE ( 'NONE', #7543, 28.50000000000000355 ) ;
#4801 = EDGE_CURVE ( 'NONE', #3903, #6783, #114, .T. ) ;
#4802 = EDGE_LOOP ( 'NONE', ( #7337, #1816 ) ) ;
#4803 = ADVANCED_FACE ( 'NONE', ( #5892 ), #6999, .F. ) ;
#4804 = ORIENTED_EDGE ( 'NONE', *, *, #7554, .F. ) ;
#4805 = ORIENTED_EDGE ( 'NONE', *, *, #5584, .F. ) ;
#4806 = FACE_OUTER_BOUND ( 'NONE', #4090, .T. ) ;
#4807 = PRESENTATION_STYLE_ASSIGNMENT (( #2419 ) ) ;
#4808 = DIRECTION ( 'NONE',  ( -0.000000000000000000, -0.000000000000000000, 1.000000000000000000 ) ) ;
#4809 = EDGE_CURVE ( 'NONE', #3008, #3595, #4775, .T. ) ;
#4810 = EDGE_LOOP ( 'NONE', ( #4015, #2392, #34, #7 ) ) ;
#4811 = ORIENTED_EDGE ( 'NONE', *, *, #3266, .F. ) ;
#4812 = AXIS2_PLACEMENT_3D ( 'NONE', #5577, #796, #5615 ) ;
#4813 = DIRECTION ( 'NONE',  ( -0.000000000000000000, -0.000000000000000000, 1.000000000000000000 ) ) ;
#4814 = CYLINDRICAL_SURFACE ( 'NONE', #1233, 5.250000000000004441 ) ;
#4815 = CARTESIAN_POINT ( 'NONE',  ( -63.51644452187023404, -49.96174644486060856, 10.00000000000000000 ) ) ;
#4816 = CIRCLE ( 'NONE', #1806, 29.99999999999999289 ) ;
#4817 = B_SPLINE_CURVE_WITH_KNOTS ( 'NONE', 3,
 ( #1388, #7533, #3802, #6204, #790, #5647, #3209, #5612 ),
 .UNSPECIFIED., .F., .F.,
 ( 4, 2, 2, 4 ),
 ( 0.004673709593152153112, 0.005837709341827643401, 0.007001709090503132824, 0.009329708587854111668 ),
 .UNSPECIFIED. ) ;
#4818 = ORIENTED_EDGE ( 'NONE', *, *, #5446, .T. ) ;
#4819 = AXIS2_PLACEMENT_3D ( 'NONE', #517, #3436, #1706 ) ;
#4820 = EDGE_CURVE ( 'NONE', #185, #3544, #3333, .T. ) ;
#4821 = ORIENTED_EDGE ( 'NONE', *, *, #5302, .F. ) ;
#4822 = DIRECTION ( 'NONE',  ( 1.000000000000000000, 0.000000000000000000, 0.000000000000000000 ) ) ;
#4823 = CARTESIAN_POINT ( 'NONE',  ( 21.01644452187054313, 80.83980388508807380, 0.000000000000000000 ) ) ;
#4824 = AXIS2_PLACEMENT_3D ( 'NONE', #7385, #6131, #4979 ) ;
#4825 = CARTESIAN_POINT ( 'NONE',  ( 0.000000000000000000, 0.000000000000000000, -50.00000000000000000 ) ) ;
#4826 = DIRECTION ( 'NONE',  ( 1.000000000000000000, 0.000000000000000000, 0.000000000000000000 ) ) ;
#4827 = ITEM_DEFINED_TRANSFORMATION ( 'NONE', 'NONE', #4222,  #7485 ) ;
#4828 = DIRECTION ( 'NONE',  ( 1.000000000000000000, 0.000000000000000000, 0.000000000000000000 ) ) ;
#4829 = ORIENTED_EDGE ( 'NONE', *, *, #5486, .F. ) ;
#4830 = FACE_OUTER_BOUND ( 'NONE', #1682, .T. ) ;
#4831 = CARTESIAN_POINT ( 'NONE',  ( 0.000000000000000000, 1.484218055610305731, 0.000000000000000000 ) ) ;
#4832 = DIRECTION ( 'NONE',  ( 0.000000000000000000, 0.000000000000000000, 1.000000000000000000 ) ) ;
#4833 = DIRECTION ( 'NONE',  ( -4.649428319898515417E-17, 1.849298671161509305E-17, -0.9999999999999998890 ) ) ;
#4834 = AXIS2_PLACEMENT_3D ( 'NONE', #4679, #4167, #2799 ) ;
#4835 = CARTESIAN_POINT ( 'NONE',  ( 105.4635834177251326, -106.6650485055556601, 0.000000000000000000 ) ) ;
#4836 = DIRECTION ( 'NONE',  ( -0.000000000000000000, -0.000000000000000000, -1.000000000000000000 ) ) ;
#4837 = FACE_BOUND ( 'NONE', #5628, .T. ) ;
#4838 = ORIENTED_EDGE ( 'NONE', *, *, #6365, .F. ) ;
#4839 = ORIENTED_EDGE ( 'NONE', *, *, #1344, .F. ) ;
#4840 = VECTOR ( 'NONE', #5304, 1000.000000000000000 ) ;
#4841 =( GEOMETRIC_REPRESENTATION_CONTEXT ( 3 ) GLOBAL_UNCERTAINTY_ASSIGNED_CONTEXT ( ( #6659 ) ) GLOBAL_UNIT_ASSIGNED_CONTEXT ( ( #6276, #1379, #2063 ) ) REPRESENTATION_CONTEXT ( 'NONE', 'WORKASPACE' ) );
#4842 = ORIENTED_EDGE ( 'NONE', *, *, #5089, .T. ) ;
#4843 = DIRECTION ( 'NONE',  ( -0.000000000000000000, -0.000000000000000000, -1.000000000000000000 ) ) ;
#4844 = CARTESIAN_POINT ( 'NONE',  ( 4.000000000000005329, -6.928203230275506108, -4.700000000000000178 ) ) ;
#4845 = CARTESIAN_POINT ( 'NONE',  ( -10.00000000000000000, 0.000000000000000000, -60.00000000000000711 ) ) ;
#4846 = AXIS2_PLACEMENT_3D ( 'NONE', #5347, #998, #403 ) ;
#4847 = PRODUCT_DEFINITION_SHAPE ( 'NONE', 'NONE',  #7792 ) ;
#4848 = ORIENTED_EDGE ( 'NONE', *, *, #6009, .F. ) ;
#4849 = ORIENTED_EDGE ( 'NONE', *, *, #5089, .F. ) ;
#4850 = EDGE_CURVE ( 'NONE', #115, #5419, #1766, .T. ) ;
#4851 = AXIS2_PLACEMENT_3D ( 'NONE', #1567, #4605, #5868 ) ;
#4852 = CYLINDRICAL_SURFACE ( 'NONE', #4287, 4.999999999999990230 ) ;
#4853 = EDGE_CURVE ( 'NONE', #6904, #3662, #983, .T. ) ;
#4854 = DIRECTION ( 'NONE',  ( -0.000000000000000000, -0.000000000000000000, 1.000000000000000000 ) ) ;
#4855 = CARTESIAN_POINT ( 'NONE',  ( 0.000000000000000000, 0.000000000000000000, 10.00000000000000888 ) ) ;
#4856 = EDGE_LOOP ( 'NONE', ( #7611, #4751, #7649, #1101 ) ) ;
#4857 = EDGE_CURVE ( 'NONE', #3320, #736, #7299, .T. ) ;
#4858 = ADVANCED_FACE ( 'NONE', ( #1635 ), #1553, .F. ) ;
#4859 = VERTEX_POINT ( 'NONE', #5262 ) ;
#4860 = DIRECTION ( 'NONE',  ( 1.000000000000000000, 0.000000000000000000, 0.000000000000000000 ) ) ;
#4861 = LINE ( 'NONE', #7349, #928 ) ;
#4862 = DIRECTION ( 'NONE',  ( 1.000000000000000000, 0.000000000000000000, 0.000000000000000000 ) ) ;
#4863 = DIRECTION ( 'NONE',  ( 0.000000000000000000, 0.000000000000000000, 1.000000000000000000 ) ) ;
#4864 = ADVANCED_FACE ( 'NONE', ( #7664 ), #4074, .T. ) ;
#4865 = UNCERTAINTY_MEASURE_WITH_UNIT (LENGTH_MEASURE( 1.000000000000000082E-05 ), #5273, 'distance_accuracy_value', 'NONE');
#4866 = CARTESIAN_POINT ( 'NONE',  ( 119.9981648402866341, 207.8429183184022122, -120.0000000000000000 ) ) ;
#4867 = EDGE_CURVE ( 'NONE', #3881, #1325, #4112, .T. ) ;
#4868 = ORIENTED_EDGE ( 'NONE', *, *, #369, .T. ) ;
#4869 = VECTOR ( 'NONE', #3722, 1000.000000000000000 ) ;
#4870 = CARTESIAN_POINT ( 'NONE',  ( -3.500000000000007105, 32.25000000000000000, 0.000000000000000000 ) ) ;
#4871 = CIRCLE ( 'NONE', #1471, 5.250000000000004441 ) ;
#4872 = DIRECTION ( 'NONE',  ( 1.000000000000000000, 0.000000000000000000, 0.000000000000000000 ) ) ;
#4873 = LINE ( 'NONE', #2522, #842 ) ;
#4874 = CARTESIAN_POINT ( 'NONE',  ( -4.857225732735059864E-13, 239.9963296805737798, -124.7000000000000028 ) ) ;
#4875 = PRESENTATION_STYLE_ASSIGNMENT (( #584 ) ) ;
#4876 = DIRECTION ( 'NONE',  ( -0.5000000000000037748, 0.8660254037844364872, 0.000000000000000000 ) ) ;
#4877 = PLANE ( 'NONE',  #4323 ) ;
#4878 = ORIENTED_EDGE ( 'NONE', *, *, #4271, .T. ) ;
#4879 = AXIS2_PLACEMENT_3D ( 'NONE', #4549, #6926, #7471 ) ;
#4880 = EDGE_LOOP ( 'NONE', ( #4681, #4533, #2103 ) ) ;
#4881 = UNCERTAINTY_MEASURE_WITH_UNIT (LENGTH_MEASURE( 1.000000000000000082E-05 ), #5796, 'distance_accuracy_value', 'NONE');
#4882 = ORIENTED_EDGE ( 'NONE', *, *, #5769, .F. ) ;
#4883 = DIRECTION ( 'NONE',  ( 1.000000000000000000, 0.000000000000000000, 0.000000000000000000 ) ) ;
#4884 =( NAMED_UNIT ( * ) SI_UNIT ( $, .STERADIAN. ) SOLID_ANGLE_UNIT ( ) );
#4885 = AXIS2_PLACEMENT_3D ( 'NONE', #3324, #2114, #2035 ) ;
#4886 = CARTESIAN_POINT ( 'NONE',  ( 202.5929183184021269, 119.9981648402868331, -50.00000000000000000 ) ) ;
#4887 = EDGE_LOOP ( 'NONE', ( #69, #4714, #3007, #3633 ) ) ;
#4888 = ORIENTED_EDGE ( 'NONE', *, *, #2998, .T. ) ;
#4889 = VECTOR ( 'NONE', #7029, 1000.000000000000114 ) ;
#4890 = FACE_OUTER_BOUND ( 'NONE', #3048, .T. ) ;
#4891 =( NAMED_UNIT ( * ) PLANE_ANGLE_UNIT ( ) SI_UNIT ( $, .RADIAN. ) );
#4892 = AXIS2_PLACEMENT_3D ( 'NONE', #5310, #2249, #2911 ) ;
#4893 = EDGE_CURVE ( 'NONE', #1337, #3469, #2520, .T. ) ;
#4894 = CARTESIAN_POINT ( 'NONE',  ( -3.318518101603016746, -7.321656987762879432, -1.128247885742728249E-15 ) ) ;
#4895 = CARTESIAN_POINT ( 'NONE',  ( 31.51644452187053602, 80.83980388508807380, 10.00000000000000000 ) ) ;
#4896 = EDGE_CURVE ( 'NONE', #3873, #5664, #2397, .T. ) ;
#4897 = ORIENTED_EDGE ( 'NONE', *, *, #4037, .T. ) ;
#4898 = EDGE_CURVE ( 'NONE', #3050, #4200, #6414, .T. ) ;
#4899 = AXIS2_PLACEMENT_3D ( 'NONE', #6277, #2145, #3981 ) ;
#4900 = ADVANCED_FACE ( 'NONE', ( #4269, #7198, #1876, #6682, #6092, #4567 ), #1272, .F. ) ;
#4901 = ORIENTED_EDGE ( 'NONE', *, *, #4138, .T. ) ;
#4902 = DIRECTION ( 'NONE',  ( 0.000000000000000000, 0.000000000000000000, -1.000000000000000000 ) ) ;
#4903 = DIRECTION ( 'NONE',  ( -1.000000000000000000, 0.000000000000000000, 0.000000000000000000 ) ) ;
#4904 = CARTESIAN_POINT ( 'NONE',  ( -1.852913429037944315, 300.0000000000000568, -1041.954445729288636 ) ) ;
#4905 = CARTESIAN_POINT ( 'NONE',  ( -20.63749999999999574, 0.000000000000000000, -37.50000000000000000 ) ) ;
#4906 = ITEM_DEFINED_TRANSFORMATION ( 'NONE', 'NONE', #3191,  #7485 ) ;
#4907 = CIRCLE ( 'NONE', #5535, 32.25000000000000000 ) ;
#4908 = DIRECTION ( 'NONE',  ( 1.000000000000000000, 0.000000000000000000, 0.000000000000000000 ) ) ;
#4909 = ADVANCED_FACE ( 'NONE', ( #7238 ), #3020, .F. ) ;
#4910 = EDGE_LOOP ( 'NONE', ( #4715, #7484, #2090, #1056 ) ) ;
#4911 = LINE ( 'NONE', #1317, #4185 ) ;
#4912 = DIRECTION ( 'NONE',  ( -0.000000000000000000, -0.000000000000000000, 1.000000000000000000 ) ) ;
#4913 = DIRECTION ( 'NONE',  ( -1.000000000000000000, -0.000000000000000000, -0.000000000000000000 ) ) ;
#4914 = CARTESIAN_POINT ( 'NONE',  ( 207.8429183184021269, 119.9981648402868331, -54.70000000000000284 ) ) ;
#4915 = PRODUCT_DEFINITION_SHAPE ( 'NONE', 'NONE',  #7798 ) ;
#4916 = FACE_BOUND ( 'NONE', #4958, .T. ) ;
#4918 = AXIS2_PLACEMENT_3D ( 'NONE', #4573, #1574, #346 ) ;
#4917 = DIRECTION ( 'NONE',  ( -0.000000000000000000, -0.000000000000000000, 1.000000000000000000 ) ) ;
#4919 = VERTEX_POINT ( 'NONE', #6055 ) ;
#4920 = EDGE_LOOP ( 'NONE', ( #5888, #6043, #6299, #2013 ) ) ;
#4921 = ORIENTED_EDGE ( 'NONE', *, *, #369, .F. ) ;
#4922 = CIRCLE ( 'NONE', #7062, 1.250000000000000222 ) ;
#4923 = LINE ( 'NONE', #1857, #6438 ) ;
#4924 = CARTESIAN_POINT ( 'NONE',  ( -68.76644452187072432, 49.96174644486006855, -135.0000000000000000 ) ) ;
#4925 = ORIENTED_EDGE ( 'NONE', *, *, #2453, .T. ) ;
#4926 = ORIENTED_EDGE ( 'NONE', *, *, #4259, .T. ) ;
#4927 = ORIENTED_EDGE ( 'NONE', *, *, #982, .T. ) ;
#4928 = DIRECTION ( 'NONE',  ( -1.000000000000000000, 0.000000000000000000, -0.000000000000000000 ) ) ;
#4929 = CARTESIAN_POINT ( 'NONE',  ( -8.000000000000001776, -1.555946510856144105, -4.632911297836646014 ) ) ;
#4930 = CARTESIAN_POINT ( 'NONE',  ( 199.9963296805737230, -4.796075449120964792E-12, 576.0908266162076643 ) ) ;
#4931 = DIRECTION ( 'NONE',  ( 1.000000000000000000, 0.000000000000000000, 0.000000000000000000 ) ) ;
#4932 = ORIENTED_EDGE ( 'NONE', *, *, #1778, .T. ) ;
#4933 = B_SPLINE_CURVE_WITH_KNOTS ( 'NONE', 3,
 ( #6383, #6268, #300, #2135, #4563, #1566 ),
 .UNSPECIFIED., .F., .F.,
 ( 4, 2, 4 ),
 ( 0.01291313371729457642, 0.01525081363757308656, 0.01758849355785159843 ),
 .UNSPECIFIED. ) ;
#4934 = AXIS2_PLACEMENT_3D ( 'NONE', #5845, #2153, #4543 ) ;
#4935 = ORIENTED_EDGE ( 'NONE', *, *, #1003, .T. ) ;
#4936 = PLANE ( 'NONE',  #3239 ) ;
#4937 = DIRECTION ( 'NONE',  ( 0.000000000000000000, 0.000000000000000000, -1.000000000000000000 ) ) ;
#4938 = DIRECTION ( 'NONE',  ( -1.000000000000000000, 0.000000000000000000, 0.000000000000000000 ) ) ;
#4939 = CARTESIAN_POINT ( 'NONE',  ( 0.000000000000000000, 0.000000000000000000, 10.00000000000000000 ) ) ;
#4940 = AXIS2_PLACEMENT_3D ( 'NONE', #6986, #1616, #3947 ) ;
#4941 = EDGE_CURVE ( 'NONE', #5285, #7680, #1800, .T. ) ;
#4942 = AXIS2_PLACEMENT_3D ( 'NONE', #1849, #6656, #6068 ) ;
#4943 = DIRECTION ( 'NONE',  ( 1.000000000000000000, 0.000000000000000000, 0.000000000000000000 ) ) ;
#4944 = ORIENTED_EDGE ( 'NONE', *, *, #6164, .T. ) ;
#4945 = VECTOR ( 'NONE', #6468, 1000.000000000000000 ) ;
#4946 = DIRECTION ( 'NONE',  ( 0.000000000000000000, 0.000000000000000000, 1.000000000000000000 ) ) ;
#4947 = EDGE_CURVE ( 'NONE', #4221, #3469, #4233, .T. ) ;
#4948 = CARTESIAN_POINT ( 'NONE',  ( 1.469553684752138043E-14, 239.9963296805737230, 10.00000000000000178 ) ) ;
#4949 = CARTESIAN_POINT ( 'NONE',  ( -1.728922298134113098E-15, 8.513302795252935035E-16, 13.00000000000000178 ) ) ;
#4950 = DIRECTION ( 'NONE',  ( -1.127550299657588165E-16, 1.986689872246140856E-17, 0.9999999999999998890 ) ) ;
#4951 = SURFACE_STYLE_USAGE ( .BOTH. , #4321 ) ;
#4952 = DIRECTION ( 'NONE',  ( -0.000000000000000000, -0.000000000000000000, 1.000000000000000000 ) ) ;
#4953 = CIRCLE ( 'NONE', #4824, 29.99999999999999289 ) ;
#4954 = DIRECTION ( 'NONE',  ( -0.000000000000000000, -0.000000000000000000, 1.000000000000000000 ) ) ;
#4955 = ORIENTED_EDGE ( 'NONE', *, *, #2017, .F. ) ;
#4956 = ORIENTED_EDGE ( 'NONE', *, *, #4559, .F. ) ;
#4957 = EDGE_CURVE ( 'NONE', #5517, #219, #4746, .T. ) ;
#4958 = EDGE_LOOP ( 'NONE', ( #3135, #5897 ) ) ;
#4959 = CIRCLE ( 'NONE', #2072, 10.00000000000000178 ) ;
#4960 = AXIS2_PLACEMENT_3D ( 'NONE', #6646, #3400, #2659 ) ;
#4961 = DIRECTION ( 'NONE',  ( 1.000000000000000000, 0.000000000000000000, 0.000000000000000000 ) ) ;
#4962 = SURFACE_SIDE_STYLE ('',( #5074 ) ) ;
#4963 = CARTESIAN_POINT ( 'NONE',  ( -3.199999999999994404, 4.592425496802574367E-15, 37.50000000000000000 ) ) ;
#4964 = EDGE_CURVE ( 'NONE', #3320, #7398, #3099, .T. ) ;
#4965 = EDGE_LOOP ( 'NONE', ( #5035, #551 ) ) ;
#4966 = AXIS2_PLACEMENT_3D ( 'NONE', #6937, #228, #6269 ) ;
#4967 = ORIENTED_EDGE ( 'NONE', *, *, #1871, .F. ) ;
#4968 = CIRCLE ( 'NONE', #1430, 40.00000000000000711 ) ;
#4969 = ORIENTED_EDGE ( 'NONE', *, *, #5338, .F. ) ;
#4970 = CYLINDRICAL_SURFACE ( 'NONE', #2156, 199.9963296805737230 ) ;
#4971 = VECTOR ( 'NONE', #3891, 1000.000000000000000 ) ;
#4972 = COLOUR_RGB ( '',0.8941176470588234615, 0.8941176470588234615, 0.8941176470588234615 ) ;
#4973 = DIRECTION ( 'NONE',  ( 1.000000000000000000, 0.000000000000000000, 0.000000000000000000 ) ) ;
#4974 = ORIENTED_EDGE ( 'NONE', *, *, #3940, .T. ) ;
#4975 = AXIS2_PLACEMENT_3D ( 'NONE', #4643, #7676, #7130 ) ;
#4976 = AXIS2_PLACEMENT_3D ( 'NONE', #5702, #224, #2640 ) ;
#4977 = PRODUCT_DEFINITION_SHAPE ( 'NONE', 'NONE',  #7801 ) ;
#4978 = FACE_OUTER_BOUND ( 'NONE', #5833, .T. ) ;
#4979 = DIRECTION ( 'NONE',  ( -1.000000000000000000, -1.776356839400250465E-15, 0.000000000000000000 ) ) ;
#4980 = CYLINDRICAL_SURFACE ( 'NONE', #3762, 5.249999999999976907 ) ;
#4981 = CARTESIAN_POINT ( 'NONE',  ( -63.76644452187071721, 49.96174644486006855, -40.00000000000000000 ) ) ;
#4982 = PRODUCT_RELATED_PRODUCT_CATEGORY ( 'part', '', ( #1837 ) ) ;
#4983 = ORIENTED_EDGE ( 'NONE', *, *, #2175, .T. ) ;
#4984 = B_SPLINE_CURVE_WITH_KNOTS ( 'NONE', 3,
 ( #4094, #7762, #7722, #2258, #4173, #3470 ),
 .UNSPECIFIED., .F., .F.,
 ( 4, 2, 4 ),
 ( 0.01291313371729457642, 0.01525081363757309350, 0.01758849355785161231 ),
 .UNSPECIFIED. ) ;
#4985 = AXIS2_PLACEMENT_3D ( 'NONE', #4473, #3331, #3918 ) ;
#4986 = LINE ( 'NONE', #6289, #6137 ) ;
#4987 = FACE_OUTER_BOUND ( 'NONE', #7055, .T. ) ;
#4988 = CARTESIAN_POINT ( 'NONE',  ( 0.000000000000000000, 0.000000000000000000, -60.00000000000000000 ) ) ;
#4989 = CARTESIAN_POINT ( 'NONE',  ( 2.718977167127996086, 29.87653198021210343, 13.00000000000001066 ) ) ;
#4990 = DIRECTION ( 'NONE',  ( -1.986689872246102645E-17, -1.127550299657589151E-16, 0.9999999999999998890 ) ) ;
#4991 = AXIS2_PLACEMENT_3D ( 'NONE', #834, #7460, #4464 ) ;
#4992 = EDGE_CURVE ( 'NONE', #3424, #1191, #4786, .T. ) ;
#4993 = PLANE ( 'NONE',  #494 ) ;
#4994 = ORIENTED_EDGE ( 'NONE', *, *, #2314, .T. ) ;
#4995 = EDGE_CURVE ( 'NONE', #4081, #7680, #5909, .T. ) ;
#4996 = VERTEX_POINT ( 'NONE', #4196 ) ;
#4997 = ADVANCED_FACE ( 'NONE', ( #19 ), #1840, .T. ) ;
#4998 = ORIENTED_EDGE ( 'NONE', *, *, #6740, .F. ) ;
#4999 = CIRCLE ( 'NONE', #6642, 5.249999999999997335 ) ;
#5000 = EDGE_CURVE ( 'NONE', #1572, #5558, #7174, .T. ) ;
#5001 = VERTEX_POINT ( 'NONE', #4155 ) ;
#5002 = DIRECTION ( 'NONE',  ( -0.000000000000000000, -0.000000000000000000, 1.000000000000000000 ) ) ;
#5003 = CARTESIAN_POINT ( 'NONE',  ( 202.5929183184021269, 119.9981648402868331, 10.00000000000000178 ) ) ;
#5004 = EDGE_CURVE ( 'NONE', #1194, #6563, #4647, .T. ) ;
#5005 = CIRCLE ( 'NONE', #1602, 5.249999999999976907 ) ;
#5006 = ORIENTED_EDGE ( 'NONE', *, *, #6253, .T. ) ;
#5007 = VERTEX_POINT ( 'NONE', #4307 ) ;
#5008 = VECTOR ( 'NONE', #6528, 1000.000000000000114 ) ;
#5009 = DIRECTION ( 'NONE',  ( 1.000000000000000000, 0.000000000000000000, 0.000000000000000000 ) ) ;
#5010 = SHAPE_REPRESENTATION_RELATIONSHIP ( 'NONE' , 'NONE' ,  #637, #5187 ) ;
#5011 = ADVANCED_BREP_SHAPE_REPRESENTATION ( '', ( #5676, #7485 ), #7737 ) ;
#5012 = SHAPE_REPRESENTATION ( 'base plate', ( #7485 ), #4585 ) ;
#5013 = DIRECTION ( 'NONE',  ( 0.000000000000000000, 0.000000000000000000, -1.000000000000000000 ) ) ;
#5014 = CARTESIAN_POINT ( 'NONE',  ( 2.644994884459109574, -7.710515798486373029, -0.08224679563971952490 ) ) ;
#5015 = ORIENTED_EDGE ( 'NONE', *, *, #3261, .F. ) ;
#5016 = AXIS2_PLACEMENT_3D ( 'NONE', #3557, #1147, #5254 ) ;
#5017 = CIRCLE ( 'NONE', #1239, 5.000000000000004441 ) ;
#5018 = FACE_OUTER_BOUND ( 'NONE', #7271, .T. ) ;
#5019 = FACE_OUTER_BOUND ( 'NONE', #2454, .T. ) ;
#5020 = CARTESIAN_POINT ( 'NONE',  ( 0.000000000000000000, 0.000000000000000000, 0.000000000000000000 ) ) ;
#5021 = ITEM_DEFINED_TRANSFORMATION ( 'NONE', 'NONE', #6958,  #7485 ) ;
#5022 = CARTESIAN_POINT ( 'NONE',  ( 145.1064334105738567, -38.00161816110870916, 10.00000000000000000 ) ) ;
#5023 = ORIENTED_EDGE ( 'NONE', *, *, #4552, .T. ) ;
#5024 = AXIS2_PLACEMENT_3D ( 'NONE', #6647, #570, #1234 ) ;
#5025 = DIRECTION ( 'NONE',  ( -1.000000000000000000, 0.000000000000000000, 0.000000000000000000 ) ) ;
#5026 = CARTESIAN_POINT ( 'NONE',  ( -5.554394503829287011, 27.95350964898380752, -82.99999999999995737 ) ) ;
#5027 = AXIS2_PLACEMENT_3D ( 'NONE', #1785, #5877, #1136 ) ;
#5028 = CARTESIAN_POINT ( 'NONE',  ( 30.00000000000000355, 0.000000000000000000, 20.00000000000000000 ) ) ;
#5029 = CARTESIAN_POINT ( 'NONE',  ( 105.4635834177251326, -106.6650485055556601, 10.00000000000000000 ) ) ;
#5030 = DIRECTION ( 'NONE',  ( 1.000000000000000000, 0.000000000000000000, 0.000000000000000000 ) ) ;
#5031 = CYLINDRICAL_SURFACE ( 'NONE', #6551, 32.49999999999997158 ) ;
#5032 = EDGE_LOOP ( 'NONE', ( #4878, #1524, #5364, #2059 ) ) ;
#5033 = ORIENTED_EDGE ( 'NONE', *, *, #5446, .F. ) ;
#5034 = MECHANICAL_DESIGN_GEOMETRIC_PRESENTATION_REPRESENTATION (  '', ( #6178 ), #1384 ) ;
#5035 = ORIENTED_EDGE ( 'NONE', *, *, #7409, .F. ) ;
#5036 = ORIENTED_EDGE ( 'NONE', *, *, #3842, .T. ) ;
#5037 = CARTESIAN_POINT ( 'NONE',  ( 0.000000000000000000, 0.000000000000000000, -4.699999999999999289 ) ) ;
#5038 = LINE ( 'NONE', #2963, #5922 ) ;
#5039 = CONICAL_SURFACE ( 'NONE', #2034, 8.000000000000000000, 1.047197551196596299 ) ;
#5040 = DIRECTION ( 'NONE',  ( -0.000000000000000000, -0.000000000000000000, -1.000000000000000000 ) ) ;
#5041 = ADVANCED_FACE ( 'NONE', ( #1115, #3528, #5458, #2944, #2981, #5343, #7741 ), #3908, .F. ) ;
#5042 = PRODUCT_DEFINITION_SHAPE ( 'NONE', 'NONE',  #3786 ) ;
#5043 = ORIENTED_EDGE ( 'NONE', *, *, #2302, .T. ) ;
#5044 = ORIENTED_EDGE ( 'NONE', *, *, #5576, .F. ) ;
#5045 = AXIS2_PLACEMENT_3D ( 'NONE', #975, #1613, #7056 ) ;
#5046 = DIRECTION ( 'NONE',  ( -0.000000000000000000, -0.000000000000000000, 1.000000000000000000 ) ) ;
#5047 = EDGE_CURVE ( 'NONE', #4257, #7689, #2144, .T. ) ;
#5048 = CARTESIAN_POINT ( 'NONE',  ( -32.49999999999997158, 0.000000000000000000, -119.9999999999999858 ) ) ;
#5049 = AXIS2_PLACEMENT_3D ( 'NONE', #3862, #1448, #5666 ) ;
#5050 = LINE ( 'NONE', #4460, #2440 ) ;
#5051 = VERTEX_POINT ( 'NONE', #6719 ) ;
#5052 = CARTESIAN_POINT ( 'NONE',  ( 279.9963296805736945, -6.783120157456498832E-12, 10.00000000000000000 ) ) ;
#5053 = DIRECTION ( 'NONE',  ( 1.000000000000000000, 0.000000000000000000, 0.000000000000000000 ) ) ;
#5054 = CARTESIAN_POINT ( 'NONE',  ( -2.645508037661888689, -7.710219529346611367, -4.631901280394566278 ) ) ;
#5055 = CONTEXT_DEPENDENT_SHAPE_REPRESENTATION ( #3096, #5482 ) ;
#5056 = CARTESIAN_POINT ( 'NONE',  ( -202.5929183184026670, 119.9981648402859378, -50.00000000000000000 ) ) ;
#5057 = ADVANCED_FACE ( 'NONE', ( #1500 ), #864, .T. ) ;
#5058 = ORIENTED_EDGE ( 'NONE', *, *, #5621, .T. ) ;
#5059 = DIRECTION ( 'NONE',  ( -0.5000000000000006661, 0.8660254037844383745, 0.000000000000000000 ) ) ;
#5060 = CARTESIAN_POINT ( 'NONE',  ( 5.238334947888644955, -36.57199107895616663, 0.000000000000000000 ) ) ;
#5061 = CIRCLE ( 'NONE', #5566, 7.999999999999998224 ) ;
#5062 = LINE ( 'NONE', #7470, #911 ) ;
#5063 = DIRECTION ( 'NONE',  ( 0.8571673007021121116, 0.000000000000000000, 0.5150380749100544886 ) ) ;
#5064 = APPLICATION_PROTOCOL_DEFINITION ( 'draft international standard', 'automotive_design', 1998, #7516 ) ;
#5065 = CARTESIAN_POINT ( 'NONE',  ( 2.644994884459109574, -7.710515798486373029, -4.617753204360279362 ) ) ;
#5066 = ORIENTED_EDGE ( 'NONE', *, *, #5863, .T. ) ;
#5067 = EDGE_LOOP ( 'NONE', ( #4636, #2839, #7681, #4521 ) ) ;
#5068 = AXIS2_PLACEMENT_3D ( 'NONE', #5928, #641, #7267 ) ;
#5069 = PRODUCT_DEFINITION_FORMATION_WITH_SPECIFIED_SOURCE ( 'ANY', '', #1453, .NOT_KNOWN. ) ;
#5070 = EDGE_LOOP ( 'NONE', ( #6701, #5097 ) ) ;
#5071 = ORIENTED_EDGE ( 'NONE', *, *, #6746, .F. ) ;
#5072 = DIRECTION ( 'NONE',  ( -0.000000000000000000, -0.000000000000000000, -1.000000000000000000 ) ) ;
#5073 = DIRECTION ( 'NONE',  ( 1.000000000000000000, 0.000000000000000000, 0.000000000000000000 ) ) ;
#5074 = SURFACE_STYLE_FILL_AREA ( #7482 ) ;
#5075 = AXIS2_PLACEMENT_3D ( 'NONE', #2356, #2941, #5341 ) ;
#5076 = DIRECTION ( 'NONE',  ( 0.3566035499204626702, -0.9342558044690565389, 2.649161120199466423E-17 ) ) ;
#5077 = ORIENTED_EDGE ( 'NONE', *, *, #4559, .T. ) ;
#5078 = ORIENTED_EDGE ( 'NONE', *, *, #138, .F. ) ;
#5079 = AXIS2_PLACEMENT_3D ( 'NONE', #3197, #2533, #2421 ) ;
#5080 = ORIENTED_EDGE ( 'NONE', *, *, #560, .F. ) ;
#5081 = DIRECTION ( 'NONE',  ( 0.000000000000000000, 0.000000000000000000, 1.000000000000000000 ) ) ;
#5082 = CYLINDRICAL_SURFACE ( 'NONE', #7356, 5.249999999999976907 ) ;
#5083 = CARTESIAN_POINT ( 'NONE',  ( 0.000000000000000000, 0.000000000000000000, 33.75000000000000000 ) ) ;
#5084 = CIRCLE ( 'NONE', #2200, 8.000000000000000000 ) ;
#5085 = DIRECTION ( 'NONE',  ( 0.000000000000000000, 0.000000000000000000, -1.000000000000000000 ) ) ;
#5086 = EDGE_CURVE ( 'NONE', #3424, #2474, #6668, .T. ) ;
#5087 = EDGE_LOOP ( 'NONE', ( #3252, #6918 ) ) ;
#5088 = EDGE_CURVE ( 'NONE', #7447, #2140, #6919, .T. ) ;
#5089 = EDGE_CURVE ( 'NONE', #2430, #5275, #3390, .T. ) ;
#5090 = AXIS2_PLACEMENT_3D ( 'NONE', #5588, #1481, #5108 ) ;
#5091 = MECHANICAL_DESIGN_GEOMETRIC_PRESENTATION_REPRESENTATION (  '', ( #5219 ), #4841 ) ;
#5092 = ADVANCED_FACE ( 'NONE', ( #6765, #5533 ), #2805, .T. ) ;
#5093 = CARTESIAN_POINT ( 'NONE',  ( 3.199999999999994404, 4.592425496802574367E-15, 37.50000000000000000 ) ) ;
#5094 = CARTESIAN_POINT ( 'NONE',  ( -68.76644452187072432, 49.96174644486006855, -134.1720000000000255 ) ) ;
#5095 = DIRECTION ( 'NONE',  ( 0.000000000000000000, 0.000000000000000000, -1.000000000000000000 ) ) ;
#5096 = DIRECTION ( 'NONE',  ( 1.000000000000000000, 0.000000000000000000, 0.000000000000000000 ) ) ;
#5097 = ORIENTED_EDGE ( 'NONE', *, *, #7499, .T. ) ;
#5098 = ADVANCED_FACE ( 'NONE', ( #5716 ), #1118, .T. ) ;
#5099 = COLOUR_RGB ( '',1.000000000000000000, 0.9490196078431372140, 0.9098039215686274384 ) ;
#5100 =( REPRESENTATION_RELATIONSHIP ('NONE','NONE', #1229, #2306 ) REPRESENTATION_RELATIONSHIP_WITH_TRANSFORMATION ( #1117 )SHAPE_REPRESENTATION_RELATIONSHIP( ) );
#5101 = DIRECTION ( 'NONE',  ( -1.000000000000000000, 0.000000000000000000, 0.000000000000000000 ) ) ;
#5102 = DIRECTION ( 'NONE',  ( -0.000000000000000000, -0.000000000000000000, 1.000000000000000000 ) ) ;
#5103 = EDGE_CURVE ( 'NONE', #2925, #57, #4522, .T. ) ;
#5104 = CARTESIAN_POINT ( 'NONE',  ( 1.469553684752138043E-14, 239.9963296805737230, -8.673617379884035472E-15 ) ) ;
#5105 = CARTESIAN_POINT ( 'NONE',  ( 30.00000000000000000, 0.000000000000000000, 0.000000000000000000 ) ) ;
#5106 = CARTESIAN_POINT ( 'NONE',  ( 0.000000000000000000, 0.000000000000000000, 3.859999999999999876 ) ) ;
#5107 = ITEM_DEFINED_TRANSFORMATION ( 'NONE', 'NONE', #2594,  #7485 ) ;
#5108 = DIRECTION ( 'NONE',  ( 0.000000000000000000, -1.000000000000000000, 0.000000000000000000 ) ) ;
#5109 = ORIENTED_EDGE ( 'NONE', *, *, #6848, .T. ) ;
#5110 = AXIS2_PLACEMENT_3D ( 'NONE', #284, #7503, #841 ) ;
#5111 = EDGE_LOOP ( 'NONE', ( #2439, #1297 ) ) ;
#5112 = EDGE_LOOP ( 'NONE', ( #7202, #1171, #5438, #4774 ) ) ;
#5113 = VERTEX_POINT ( 'NONE', #310 ) ;
#5114 = CIRCLE ( 'NONE', #2106, 150.0000000000000568 ) ;
#5115 = CARTESIAN_POINT ( 'NONE',  ( 4.000000000000004441, 6.928203230275507885, 0.000000000000000000 ) ) ;
#5116 = DIRECTION ( 'NONE',  ( -5.551115123125782702E-17, 0.000000000000000000, -1.000000000000000000 ) ) ;
#5117 = CARTESIAN_POINT ( 'NONE',  ( -10.00000000000000000, 33.54101966249685773, -60.00000000000000711 ) ) ;
#5118 = ORIENTED_EDGE ( 'NONE', *, *, #191, .T. ) ;
#5119 = AXIS2_PLACEMENT_3D ( 'NONE', #245, #875, #840 ) ;
#5120 = VERTEX_POINT ( 'NONE', #6985 ) ;
#5121 = VERTEX_POINT ( 'NONE', #3139 ) ;
#5122 = CARTESIAN_POINT ( 'NONE',  ( 26.26644452187053957, 80.83980388508807380, 10.00000000000000000 ) ) ;
#5123 = CIRCLE ( 'NONE', #6139, 0.7500000000000041078 ) ;
#5124 = DIRECTION ( 'NONE',  ( 1.000000000000000000, 0.000000000000000000, 0.000000000000000000 ) ) ;
#5125 = DIRECTION ( 'NONE',  ( -0.000000000000000000, -0.000000000000000000, 1.000000000000000000 ) ) ;
#5126 = ORIENTED_EDGE ( 'NONE', *, *, #2316, .T. ) ;
#5127 = CIRCLE ( 'NONE', #3879, 37.50000000000000000 ) ;
#5128 = EDGE_CURVE ( 'NONE', #3378, #5120, #5590, .T. ) ;
#5129 = CARTESIAN_POINT ( 'NONE',  ( 0.000000000000000000, 0.000000000000000000, -79.99999999999995737 ) ) ;
#5130 = DIRECTION ( 'NONE',  ( -0.000000000000000000, -0.000000000000000000, -1.000000000000000000 ) ) ;
#5131 = FACE_OUTER_BOUND ( 'NONE', #6531, .T. ) ;
#5132 = EDGE_CURVE ( 'NONE', #2245, #7440, #722, .T. ) ;
#5133 = EDGE_CURVE ( 'NONE', #2129, #7603, #5463, .T. ) ;
#5134 = AXIS2_PLACEMENT_3D ( 'NONE', #1225, #4301, #6709 ) ;
#5135 = DIRECTION ( 'NONE',  ( 1.000000000000000000, 0.000000000000000000, 0.000000000000000000 ) ) ;
#5136 = EDGE_LOOP ( 'NONE', ( #230, #2763, #4048, #2010 ) ) ;
#5137 = ADVANCED_FACE ( 'NONE', ( #3280 ), #676, .T. ) ;
#5138 = PLANE ( 'NONE',  #6011 ) ;
#5139 = AXIS2_PLACEMENT_3D ( 'NONE', #135, #7528, #4349 ) ;
#5140 = CARTESIAN_POINT ( 'NONE',  ( 279.9963296805736945, -6.783120157456498832E-12, 10.00000000000000000 ) ) ;
#5141 = CARTESIAN_POINT ( 'NONE',  ( 28.49999999999999645, 0.000000000000000000, 0.000000000000000000 ) ) ;
#5142 = DIRECTION ( 'NONE',  ( -0.000000000000000000, 0.000000000000000000, -1.000000000000000000 ) ) ;
#5143 = CYLINDRICAL_SURFACE ( 'NONE', #5756, 4.999999999999990230 ) ;
#5144 = CONTEXT_DEPENDENT_SHAPE_REPRESENTATION ( #5911, #4282 ) ;
#5145 = ADVANCED_FACE ( 'NONE', ( #269 ), #1311, .F. ) ;
#5146 = VECTOR ( 'NONE', #4242, 1000.000000000000000 ) ;
#5147 = ORIENTED_EDGE ( 'NONE', *, *, #4317, .T. ) ;
#5148 = ORIENTED_EDGE ( 'NONE', *, *, #2507, .T. ) ;
#5149 = EDGE_LOOP ( 'NONE', ( #4039, #5148, #78, #184 ) ) ;
#5150 = AXIS2_PLACEMENT_3D ( 'NONE', #401, #7074, #5773 ) ;
#5151 = ORIENTED_EDGE ( 'NONE', *, *, #5761, .F. ) ;
#5152 = LINE ( 'NONE', #1153, #1941 ) ;
#5153 = LINE ( 'NONE', #4367, #5646 ) ;
#5154 = CARTESIAN_POINT ( 'NONE',  ( -3.200000000000008171, 0.000000000000000000, -30.00000000000000000 ) ) ;
#5155 = LINE ( 'NONE', #3388, #3584 ) ;
#5156 = AXIS2_PLACEMENT_3D ( 'NONE', #2299, #3512, #4685 ) ;
#5157 = ORIENTED_EDGE ( 'NONE', *, *, #1138, .T. ) ;
#5158 = ORIENTED_EDGE ( 'NONE', *, *, #4613, .F. ) ;
#5159 = ORIENTED_EDGE ( 'NONE', *, *, #2368, .T. ) ;
#5160 = VECTOR ( 'NONE', #5116, 1000.000000000000000 ) ;
#5161 = CARTESIAN_POINT ( 'NONE',  ( -20.63749999999999574, 0.000000000000000000, -35.97500000000000853 ) ) ;
#5162 = DIRECTION ( 'NONE',  ( 0.000000000000000000, 0.000000000000000000, 1.000000000000000000 ) ) ;
#5163 = B_SPLINE_CURVE_WITH_KNOTS ( 'NONE', 3,
 ( #2562, #5542, #844, #2125, #142, #177 ),
 .UNSPECIFIED., .F., .F.,
 ( 4, 2, 4 ),
 ( 0.01291313371729457815, 0.01525081363757309523, 0.01758849355785161231 ),
 .UNSPECIFIED. ) ;
#5164 = DIRECTION ( 'NONE',  ( -0.000000000000000000, -0.000000000000000000, 1.000000000000000000 ) ) ;
#5165 = VERTEX_POINT ( 'NONE', #7606 ) ;
#5166 = VECTOR ( 'NONE', #7415, 1000.000000000000000 ) ;
#5167 = DIRECTION ( 'NONE',  ( 1.224646799147352961E-16, 1.000000000000000000, -0.000000000000000000 ) ) ;
#5168 = FACE_OUTER_BOUND ( 'NONE', #7736, .T. ) ;
#5169 = VECTOR ( 'NONE', #4684, 1000.000000000000000 ) ;
#5170 = CARTESIAN_POINT ( 'NONE',  ( 0.6543471694412381634, 8.859816792613644409, -4.203584543331201573 ) ) ;
#5171 = CARTESIAN_POINT ( 'NONE',  ( -207.8429183184020985, 119.9981648402869467, 10.00000000000000000 ) ) ;
#5172 = ORIENTED_EDGE ( 'NONE', *, *, #2167, .F. ) ;
#5173 = ADVANCED_FACE ( 'NONE', ( #1953 ), #5082, .F. ) ;
#5174 = VECTOR ( 'NONE', #6024, 1000.000000000000000 ) ;
#5175 = CARTESIAN_POINT ( 'NONE',  ( -78.76644452187068168, 49.96174644486002592, 0.000000000000000000 ) ) ;
#5176 = DIRECTION ( 'NONE',  ( 0.000000000000000000, 0.000000000000000000, 1.000000000000000000 ) ) ;
#5177 = ADVANCED_FACE ( 'NONE', ( #348 ), #2766, .F. ) ;
#5178 = FACE_OUTER_BOUND ( 'NONE', #6855, .T. ) ;
#5179 = DIRECTION ( 'NONE',  ( -1.000000000000000000, 0.000000000000000000, 0.000000000000000000 ) ) ;
#5180 = CONTEXT_DEPENDENT_SHAPE_REPRESENTATION ( #6827, #3285 ) ;
#5181 = FACE_OUTER_BOUND ( 'NONE', #4345, .T. ) ;
#5182 = ORIENTED_EDGE ( 'NONE', *, *, #3459, .T. ) ;
#5183 = VERTEX_POINT ( 'NONE', #2301 ) ;
#5184 = ORIENTED_EDGE ( 'NONE', *, *, #905, .F. ) ;
#5185 = EDGE_CURVE ( 'NONE', #1814, #2827, #1099, .T. ) ;
#5186 = AXIS2_PLACEMENT_3D ( 'NONE', #1844, #3684, #6095 ) ;
#5187 = ADVANCED_BREP_SHAPE_REPRESENTATION ( '', ( #5726, #7485 ), #2086 ) ;
#5188 = EDGE_LOOP ( 'NONE', ( #3441, #3475, #1083, #6863 ) ) ;
#5189 = CARTESIAN_POINT ( 'NONE',  ( -20.63749999999999929, 3.673940397442059178E-15, 30.00000000000000000 ) ) ;
#5190 = ADVANCED_FACE ( 'NONE', ( #7140 ), #2382, .T. ) ;
#5191 = DIRECTION ( 'NONE',  ( 0.000000000000000000, 0.000000000000000000, 1.000000000000000000 ) ) ;
#5192 = CARTESIAN_POINT ( 'NONE',  ( 0.000000000000000000, 0.000000000000000000, -4.700000000000000178 ) ) ;
#5193 = DIRECTION ( 'NONE',  ( 0.000000000000000000, 0.000000000000000000, 1.000000000000000000 ) ) ;
#5194 = FACE_OUTER_BOUND ( 'NONE', #7511, .T. ) ;
#5195 = AXIS2_PLACEMENT_3D ( 'NONE', #4855, #1794, #6599 ) ;
#5196 = CYLINDRICAL_SURFACE ( 'NONE', #5962, 31.52499999999999858 ) ;
#5197 = ORIENTED_EDGE ( 'NONE', *, *, #463, .T. ) ;
#5198 = EDGE_CURVE ( 'NONE', #2140, #4648, #3323, .T. ) ;
#5199 = ORIENTED_EDGE ( 'NONE', *, *, #2929, .T. ) ;
#5200 = ORIENTED_EDGE ( 'NONE', *, *, #3561, .F. ) ;
#5201 = VECTOR ( 'NONE', #2980, 1000.000000000000000 ) ;
#5202 = CARTESIAN_POINT ( 'NONE',  ( 30.00000000000000000, 0.000000000000000000, 0.000000000000000000 ) ) ;
#5203 = ADVANCED_FACE ( 'NONE', ( #4136 ), #1060, .F. ) ;
#5204 = DIRECTION ( 'NONE',  ( -0.000000000000000000, -0.000000000000000000, 1.000000000000000000 ) ) ;
#5205 =( REPRESENTATION_RELATIONSHIP ('NONE','NONE', #1229, #2306 ) REPRESENTATION_RELATIONSHIP_WITH_TRANSFORMATION ( #2480 )SHAPE_REPRESENTATION_RELATIONSHIP( ) );
#5206 = CARTESIAN_POINT ( 'NONE',  ( 4.250000000000000000, 0.000000000000000000, 2.573333333332999739 ) ) ;
#5207 = VECTOR ( 'NONE', #7021, 1000.000000000000000 ) ;
#5208 = ORIENTED_EDGE ( 'NONE', *, *, #7082, .T. ) ;
#5209 = ORIENTED_EDGE ( 'NONE', *, *, #7310, .T. ) ;
#5210 = DIRECTION ( 'NONE',  ( 1.000000000000000000, 0.000000000000000000, 0.000000000000000000 ) ) ;
#5211 = DIRECTION ( 'NONE',  ( -1.000000000000000000, 0.000000000000000000, 0.000000000000000000 ) ) ;
#5212 =( GEOMETRIC_REPRESENTATION_CONTEXT ( 3 ) GLOBAL_UNCERTAINTY_ASSIGNED_CONTEXT ( ( #4865 ) ) GLOBAL_UNIT_ASSIGNED_CONTEXT ( ( #5273, #6425, #4606 ) ) REPRESENTATION_CONTEXT ( 'NONE', 'WORKASPACE' ) );
#5213 = CIRCLE ( 'NONE', #7105, 35.00000000000000711 ) ;
#5214 = DIRECTION ( 'NONE',  ( -0.000000000000000000, -0.000000000000000000, 1.000000000000000000 ) ) ;
#5215 = DIRECTION ( 'NONE',  ( 0.000000000000000000, 0.000000000000000000, 1.000000000000000000 ) ) ;
#5216 = VERTEX_POINT ( 'NONE', #6552 ) ;
#5217 = ORIENTED_EDGE ( 'NONE', *, *, #2167, .T. ) ;
#5218 = AXIS2_PLACEMENT_3D ( 'NONE', #2710, #2128, #2162 ) ;
#5219 = STYLED_ITEM ( 'NONE', ( #7453 ), #1719 ) ;
#5220 = CARTESIAN_POINT ( 'NONE',  ( -4.000000000000004441, -6.928203230275506108, 0.000000000000000000 ) ) ;
#5221 = CARTESIAN_POINT ( 'NONE',  ( 10.00000000000000000, 0.000000000000000000, 10.00000000000000000 ) ) ;
#5222 = CARTESIAN_POINT ( 'NONE',  ( 85.00000000000000000, 9.720002580593245511E-13, 10.00000000000000000 ) ) ;
#5223 = DIRECTION ( 'NONE',  ( -0.000000000000000000, -0.000000000000000000, 1.000000000000000000 ) ) ;
#5224 = AXIS2_PLACEMENT_3D ( 'NONE', #2823, #2281, #1556 ) ;
#5225 = COLOUR_RGB ( '',0.8941176470588234615, 0.8941176470588234615, 0.8941176470588234615 ) ;
#5226 = CYLINDRICAL_SURFACE ( 'NONE', #1315, 28.50000000000000711 ) ;
#5227 = ORIENTED_EDGE ( 'NONE', *, *, #280, .T. ) ;
#5228 = ORIENTED_EDGE ( 'NONE', *, *, #4240, .T. ) ;
#5229 = ORIENTED_EDGE ( 'NONE', *, *, #2219, .T. ) ;
#5230 = AXIS2_PLACEMENT_3D ( 'NONE', #7714, #2334, #3933 ) ;
#5231 = FACE_OUTER_BOUND ( 'NONE', #5265, .T. ) ;
#5232 = ADVANCED_FACE ( 'NONE', ( #5919 ), #4202, .T. ) ;
#5233 = DIRECTION ( 'NONE',  ( 1.000000000000000000, 0.000000000000000000, 0.000000000000000000 ) ) ;
#5234 = FACE_BOUND ( 'NONE', #4571, .T. ) ;
#5235 = FACE_OUTER_BOUND ( 'NONE', #4880, .T. ) ;
#5236 = CARTESIAN_POINT ( 'NONE',  ( 0.000000000000000000, 0.000000000000000000, 2.573333333332999739 ) ) ;
#5237 = EDGE_CURVE ( 'NONE', #5972, #7642, #4019, .T. ) ;
#5238 = EDGE_CURVE ( 'NONE', #4221, #3738, #4959, .T. ) ;
#5239 = VERTEX_POINT ( 'NONE', #3513 ) ;
#5240 = EDGE_CURVE ( 'NONE', #2220, #3664, #6469, .T. ) ;
#5241 = ORIENTED_EDGE ( 'NONE', *, *, #6979, .T. ) ;
#5242 = CIRCLE ( 'NONE', #2721, 8.000000000000000000 ) ;
#5243 = VERTEX_POINT ( 'NONE', #2845 ) ;
#5244 = PRESENTATION_STYLE_ASSIGNMENT (( #4017 ) ) ;
#5245 = EDGE_CURVE ( 'NONE', #5120, #4919, #4651, .T. ) ;
#5246 = LINE ( 'NONE', #3006, #2697 ) ;
#5247 = ADVANCED_FACE ( 'NONE', ( #5958 ), #2344, .F. ) ;
#5248 = AXIS2_PLACEMENT_3D ( 'NONE', #4347, #6052, #2476 ) ;
#5249 = LINE ( 'NONE', #1062, #4945 ) ;
#5250 = ORIENTED_EDGE ( 'NONE', *, *, #6589, .F. ) ;
#5251 = AXIS2_PLACEMENT_3D ( 'NONE', #6401, #3399, #1704 ) ;
#5252 = CARTESIAN_POINT ( 'NONE',  ( 0.000000000000000000, 0.000000000000000000, 33.75000000000000000 ) ) ;
#5253 = DIRECTION ( 'NONE',  ( -0.000000000000000000, -0.000000000000000000, 1.000000000000000000 ) ) ;
#5254 = DIRECTION ( 'NONE',  ( 1.000000000000000000, 0.000000000000000000, 0.000000000000000000 ) ) ;
#5255 = DIRECTION ( 'NONE',  ( 0.000000000000000000, 0.000000000000000000, 1.000000000000000000 ) ) ;
#5256 = ORIENTED_EDGE ( 'NONE', *, *, #1236, .F. ) ;
#5257 = VECTOR ( 'NONE', #7246, 1000.000000000000000 ) ;
#5258 = ORIENTED_EDGE ( 'NONE', *, *, #5282, .F. ) ;
#5259 = DIRECTION ( 'NONE',  ( 0.000000000000000000, 0.000000000000000000, -1.000000000000000000 ) ) ;
#5260 = CIRCLE ( 'NONE', #98, 5.250000000000004441 ) ;
#5261 = DIRECTION ( 'NONE',  ( -0.000000000000000000, -0.000000000000000000, -1.000000000000000000 ) ) ;
#5262 = CARTESIAN_POINT ( 'NONE',  ( 6.713333333332999864, 0.000000000000000000, 3.859999999999999876 ) ) ;
#5263 = DIRECTION ( 'NONE',  ( 0.000000000000000000, 0.000000000000000000, 1.000000000000000000 ) ) ;
#5264 = CARTESIAN_POINT ( 'NONE',  ( -68.76644452187068168, 49.96174644486002592, -40.00000000000000000 ) ) ;
#5265 = EDGE_LOOP ( 'NONE', ( #6640, #6262, #7403 ) ) ;
#5266 = ORIENTED_EDGE ( 'NONE', *, *, #5245, .F. ) ;
#5267 = ORIENTED_EDGE ( 'NONE', *, *, #4947, .T. ) ;
#5268 = DIRECTION ( 'NONE',  ( 1.000000000000000000, 0.000000000000000000, 0.000000000000000000 ) ) ;
#5269 = AXIS2_PLACEMENT_3D ( 'NONE', #2443, #6726, #1919 ) ;
#5270 = CARTESIAN_POINT ( 'NONE',  ( 8.000000000000000000, -1.555946510856141884, -0.06708870216335505177 ) ) ;
#5271 = DIRECTION ( 'NONE',  ( -0.000000000000000000, -0.000000000000000000, 1.000000000000000000 ) ) ;
#5272 = DIRECTION ( 'NONE',  ( 1.000000000000000000, 0.000000000000000000, 0.000000000000000000 ) ) ;
#5273 =( LENGTH_UNIT ( ) NAMED_UNIT ( * ) SI_UNIT ( .MILLI., .METRE. ) );
#5274 = DIRECTION ( 'NONE',  ( -0.000000000000000000, -0.000000000000000000, 1.000000000000000000 ) ) ;
#5275 = VERTEX_POINT ( 'NONE', #4772 ) ;
#5276 = CIRCLE ( 'NONE', #5150, 2.250000000000001776 ) ;
#5277 = ORIENTED_EDGE ( 'NONE', *, *, #3503, .T. ) ;
#5278 = ORIENTED_EDGE ( 'NONE', *, *, #3930, .T. ) ;
#5279 = CARTESIAN_POINT ( 'NONE',  ( -10.00000000000000000, 41.99999999999999289, -60.00000000000000711 ) ) ;
#5280 = DIRECTION ( 'NONE',  ( 1.000000000000000000, 0.000000000000000000, 0.000000000000000000 ) ) ;
#5281 = AXIS2_PLACEMENT_3D ( 'NONE', #2997, #5399, #5907 ) ;
#5282 = EDGE_CURVE ( 'NONE', #3664, #1428, #7181, .T. ) ;
#5283 = CARTESIAN_POINT ( 'NONE',  ( 28.49999999999999645, 0.000000000000000000, -3.000000000000000000 ) ) ;
#5284 = LINE ( 'NONE', #3356, #2567 ) ;
#5285 = VERTEX_POINT ( 'NONE', #5283 ) ;
#5286 = MECHANICAL_DESIGN_GEOMETRIC_PRESENTATION_REPRESENTATION (  '', ( #3402 ), #630 ) ;
#5287 = EDGE_CURVE ( 'NONE', #669, #3544, #3589, .T. ) ;
#5288 = ADVANCED_BREP_SHAPE_REPRESENTATION ( '', ( #5821, #7485 ), #6239 ) ;
#5289 = CARTESIAN_POINT ( 'NONE',  ( 0.000000000000000000, 0.000000000000000000, -4.700000000000000178 ) ) ;
#5290 = CARTESIAN_POINT ( 'NONE',  ( 0.000000000000000000, 0.000000000000000000, -50.00000000000000000 ) ) ;
#5291 = DIRECTION ( 'NONE',  ( 5.551115123125782702E-17, 0.000000000000000000, 1.000000000000000000 ) ) ;
#5292 = AXIS2_PLACEMENT_3D ( 'NONE', #6865, #6943, #1413 ) ;
#5293 = CARTESIAN_POINT ( 'NONE',  ( -5.554394503829287011, 27.95350964898380752, -82.99999999999995737 ) ) ;
#5294 = ORIENTED_EDGE ( 'NONE', *, *, #2368, .F. ) ;
#5295 = ORIENTED_EDGE ( 'NONE', *, *, #5761, .T. ) ;
#5296 = CARTESIAN_POINT ( 'NONE',  ( 0.000000000000000000, 0.000000000000000000, -3.000000000000000000 ) ) ;
#5297 = VECTOR ( 'NONE', #7604, 1000.000000000000000 ) ;
#5298 = CARTESIAN_POINT ( 'NONE',  ( 10.00000000000000000, 0.000000000000000000, 10.00000000000000000 ) ) ;
#5299 = PRESENTATION_STYLE_ASSIGNMENT (( #5562 ) ) ;
#5300 = DIRECTION ( 'NONE',  ( -0.000000000000000000, -0.000000000000000000, 1.000000000000000000 ) ) ;
#5301 = DIRECTION ( 'NONE',  ( 1.000000000000000000, 0.000000000000000000, 0.000000000000000000 ) ) ;
#5302 = EDGE_CURVE ( 'NONE', #185, #4264, #5246, .T. ) ;
#5303 = CONTEXT_DEPENDENT_SHAPE_REPRESENTATION ( #1579, #5990 ) ;
#5304 = DIRECTION ( 'NONE',  ( -0.000000000000000000, -0.000000000000000000, 1.000000000000000000 ) ) ;
#5305 = AXIS2_PLACEMENT_3D ( 'NONE', #3743, #2571, #4961 ) ;
#5306 = ORIENTED_EDGE ( 'NONE', *, *, #7223, .F. ) ;
#5307 = ORIENTED_EDGE ( 'NONE', *, *, #6169, .F. ) ;
#5308 = VERTEX_POINT ( 'NONE', #5409 ) ;
#5309 = DIRECTION ( 'NONE',  ( 0.000000000000000000, 0.000000000000000000, -1.000000000000000000 ) ) ;
#5310 = CARTESIAN_POINT ( 'NONE',  ( 0.000000000000000000, 0.000000000000000000, 9.480888224575629408 ) ) ;
#5311 = CARTESIAN_POINT ( 'NONE',  ( -207.8429183184026670, 119.9981648402859378, -50.00000000000000000 ) ) ;
#5312 = DIRECTION ( 'NONE',  ( -0.8090169943749422332, -0.5877852522924802425, 0.000000000000000000 ) ) ;
#5313 = FILL_AREA_STYLE_COLOUR ( '', #6233 ) ;
#5314 = CARTESIAN_POINT ( 'NONE',  ( 5.870234470492294880E-31, -4.203179568131150526E-15, -122.9999999999999716 ) ) ;
#5315 = ORIENTED_EDGE ( 'NONE', *, *, #5439, .F. ) ;
#5316 = ORIENTED_EDGE ( 'NONE', *, *, #2838, .F. ) ;
#5317 = VERTEX_POINT ( 'NONE', #5 ) ;
#5318 = LINE ( 'NONE', #5365, #2914 ) ;
#5319 = DIRECTION ( 'NONE',  ( 1.000000000000000000, 0.000000000000000000, -0.000000000000000000 ) ) ;
#5320 = CIRCLE ( 'NONE', #2934, 30.00000000000000000 ) ;
#5321 = CARTESIAN_POINT ( 'NONE',  ( -5.238334947888650284, -36.57199107895616663, -3.000000000000000000 ) ) ;
#5322 = DIRECTION ( 'NONE',  ( 0.000000000000000000, -1.000000000000000000, 0.000000000000000000 ) ) ;
#5323 = EDGE_CURVE ( 'NONE', #5752, #3121, #4615, .T. ) ;
#5324 = ORIENTED_EDGE ( 'NONE', *, *, #5538, .F. ) ;
#5325 = EDGE_LOOP ( 'NONE', ( #4049, #1094, #3966, #3973 ) ) ;
#5326 = EDGE_CURVE ( 'NONE', #154, #6339, #1614, .T. ) ;
#5327 = UNCERTAINTY_MEASURE_WITH_UNIT (LENGTH_MEASURE( 1.000000000000000082E-05 ), #4488, 'distance_accuracy_value', 'NONE');
#5328 = DIRECTION ( 'NONE',  ( 5.551115123125782702E-17, 0.000000000000000000, 1.000000000000000000 ) ) ;
#5329 = DIRECTION ( 'NONE',  ( 1.000000000000000000, 0.000000000000000000, 0.000000000000000000 ) ) ;
#5330 = ADVANCED_FACE ( 'NONE', ( #1658 ), #1332, .T. ) ;
#5331 = CARTESIAN_POINT ( 'NONE',  ( -1.734723475976807094E-15, 9.237604307034017026, -3.985468820183668104 ) ) ;
#5332 = AXIS2_PLACEMENT_3D ( 'NONE', #3610, #2794, #1839 ) ;
#5333 = FACE_OUTER_BOUND ( 'NONE', #3860, .T. ) ;
#5334 = EDGE_CURVE ( 'NONE', #5742, #3827, #1557, .T. ) ;
#5335 = VERTEX_POINT ( 'NONE', #1258 ) ;
#5336 = ADVANCED_FACE ( 'NONE', ( #7222 ), #6667, .F. ) ;
#5337 = ORIENTED_EDGE ( 'NONE', *, *, #3226, .F. ) ;
#5338 = EDGE_CURVE ( 'NONE', #736, #7389, #3076, .T. ) ;
#5339 = ORIENTED_EDGE ( 'NONE', *, *, #5240, .T. ) ;
#5340 = PRESENTATION_STYLE_ASSIGNMENT (( #1632 ) ) ;
#5341 = DIRECTION ( 'NONE',  ( 1.000000000000000000, 0.000000000000000000, 0.000000000000000000 ) ) ;
#5342 = CARTESIAN_POINT ( 'NONE',  ( -29.99999999999999289, 3.673940397442058389E-15, -139.9999999999999716 ) ) ;
#5343 = FACE_BOUND ( 'NONE', #1925, .T. ) ;
#5344 = DIRECTION ( 'NONE',  ( -0.8660254037844382635, 0.5000000000000005551, 0.000000000000000000 ) ) ;
#5345 = ITEM_DEFINED_TRANSFORMATION ( 'NONE', 'NONE', #6243,  #7485 ) ;
#5346 = EDGE_CURVE ( 'NONE', #4452, #3391, #742, .T. ) ;
#5347 = CARTESIAN_POINT ( 'NONE',  ( 0.000000000000000000, 0.000000000000000000, -112.9999999999999716 ) ) ;
#5348 = AXIS2_PLACEMENT_3D ( 'NONE', #7132, #457, #7637 ) ;
#5349 = ORIENTED_EDGE ( 'NONE', *, *, #2400, .T. ) ;
#5350 = CIRCLE ( 'NONE', #3957, 5.249999999999976907 ) ;
#5351 = EDGE_LOOP ( 'NONE', ( #6417, #3699, #6554, #2674 ) ) ;
#5352 = EDGE_CURVE ( 'NONE', #5664, #913, #4454, .T. ) ;
#5353 = CARTESIAN_POINT ( 'NONE',  ( -68.76644452187068168, 49.96174644486002592, 0.000000000000000000 ) ) ;
#5354 = CIRCLE ( 'NONE', #2468, 0.7500000000000041078 ) ;
#5355 = PLANE ( 'NONE',  #3688 ) ;
#5356 = FACE_OUTER_BOUND ( 'NONE', #5565, .T. ) ;
#5357 = DIRECTION ( 'NONE',  ( 0.6497489119555339698, -0.7601489008165438488, 0.000000000000000000 ) ) ;
#5358 = CYLINDRICAL_SURFACE ( 'NONE', #7234, 37.50000000000000000 ) ;
#5359 = FACE_OUTER_BOUND ( 'NONE', #3116, .T. ) ;
#5360 = ORIENTED_EDGE ( 'NONE', *, *, #1772, .F. ) ;
#5361 = ORIENTED_EDGE ( 'NONE', *, *, #1688, .F. ) ;
#5362 = CLOSED_SHELL ( 'NONE', ( #1842, #1864, #1250, #2683, #2020, #2786, #2352, #747, #1386, #942, #4313, #3613, #5057, #6685, #2422, #5708, #5684, #7111, #1277, #7598, #1742, #901 ) ) ;
#5363 =( REPRESENTATION_RELATIONSHIP ('NONE','NONE', #1229, #637 ) REPRESENTATION_RELATIONSHIP_WITH_TRANSFORMATION ( #4550 )SHAPE_REPRESENTATION_RELATIONSHIP( ) );
#5364 = ORIENTED_EDGE ( 'NONE', *, *, #2645, .T. ) ;
#5365 = CARTESIAN_POINT ( 'NONE',  ( -1.852913429037944315, 300.0000000000000568, -120.0000000000000000 ) ) ;
#5366 = CARTESIAN_POINT ( 'NONE',  ( -15.99999999999998934, -6.071532165918824830E-15, -4.700000000000000178 ) ) ;
#5367 = DIRECTION ( 'NONE',  ( 0.000000000000000000, 0.000000000000000000, -1.000000000000000000 ) ) ;
#5368 = ORIENTED_EDGE ( 'NONE', *, *, #4801, .F. ) ;
#5369 = AXIS2_PLACEMENT_3D ( 'NONE', #2001, #5690, #7392 ) ;
#5370 = EDGE_LOOP ( 'NONE', ( #972, #5799, #4790, #4180 ) ) ;
#5371 = CARTESIAN_POINT ( 'NONE',  ( 10.00000000000000000, 33.54101966249685773, -50.00000000000000000 ) ) ;
#5372 = DIRECTION ( 'NONE',  ( 1.000000000000000000, 0.000000000000000000, 0.000000000000000000 ) ) ;
#5373 = AXIS2_PLACEMENT_3D ( 'NONE', #7384, #2658, #3321 ) ;
#5374 = DIRECTION ( 'NONE',  ( 0.9914448613738101601, -0.1305261922200541547, 0.000000000000000000 ) ) ;
#5375 = LINE ( 'NONE', #6084, #6207 ) ;
#5376 = ORIENTED_EDGE ( 'NONE', *, *, #3180, .T. ) ;
#5377 = VERTEX_POINT ( 'NONE', #152 ) ;
#5378 = AXIS2_PLACEMENT_3D ( 'NONE', #3993, #3485, #4545 ) ;
#5379 = EDGE_CURVE ( 'NONE', #387, #599, #6974, .T. ) ;
#5380 = ORIENTED_EDGE ( 'NONE', *, *, #6197, .F. ) ;
#5381 = LINE ( 'NONE', #2432, #6129 ) ;
#5382 = CARTESIAN_POINT ( 'NONE',  ( 0.000000000000000000, 0.000000000000000000, 0.000000000000000000 ) ) ;
#5383 = EDGE_CURVE ( 'NONE', #4859, #2866, #5838, .T. ) ;
#5384 = DIRECTION ( 'NONE',  ( -0.000000000000000000, -0.000000000000000000, -1.000000000000000000 ) ) ;
#5385 = DIRECTION ( 'NONE',  ( 1.000000000000000000, 0.000000000000000000, 0.000000000000000000 ) ) ;
#5386 = CONTEXT_DEPENDENT_SHAPE_REPRESENTATION ( #5100, #4346 ) ;
#5387 = AXIS2_PLACEMENT_3D ( 'NONE', #5586, #1886, #2486 ) ;
#5388 = EDGE_CURVE ( 'NONE', #5517, #1642, #168, .T. ) ;
#5389 = DIRECTION ( 'NONE',  ( -1.000000000000000000, 0.000000000000000000, -0.000000000000000000 ) ) ;
#5390 = ORIENTED_EDGE ( 'NONE', *, *, #7187, .F. ) ;
#5391 = VERTEX_POINT ( 'NONE', #4963 ) ;
#5392 = AXIS2_PLACEMENT_3D ( 'NONE', #4939, #685, #1349 ) ;
#5393 = CARTESIAN_POINT ( 'NONE',  ( -5.000000000000000888, 6.123233995736767268E-16, -4.699999999999999289 ) ) ;
#5394 = EDGE_CURVE ( 'NONE', #5921, #4674, #667, .T. ) ;
#5395 = ADVANCED_BREP_SHAPE_REPRESENTATION ( '', ( #3183, #7485 ), #2832 ) ;
#5396 = DIRECTION ( 'NONE',  ( -0.000000000000000000, 0.000000000000000000, -1.000000000000000000 ) ) ;
#5397 = CARTESIAN_POINT ( 'NONE',  ( -114.7481648402868188, 207.8429183184021554, 10.00000000000000178 ) ) ;
#5398 = DIRECTION ( 'NONE',  ( -0.9987587364483918595, -0.04980950078059115382, 0.000000000000000000 ) ) ;
#5399 = DIRECTION ( 'NONE',  ( 0.000000000000000000, 0.000000000000000000, 1.000000000000000000 ) ) ;
#5400 = TOROIDAL_SURFACE ( 'NONE', #4127, 6.713333333332999864, 1.286666666666999914 ) ;
#5401 = VERTEX_POINT ( 'NONE', #1980 ) ;
#5402 = VERTEX_POINT ( 'NONE', #2460 ) ;
#5403 = AXIS2_PLACEMENT_3D ( 'NONE', #6333, #769, #6217 ) ;
#5404 = ORIENTED_EDGE ( 'NONE', *, *, #2316, .F. ) ;
#5405 = AXIS2_PLACEMENT_3D ( 'NONE', #865, #4457, #6868 ) ;
#5406 = DIRECTION ( 'NONE',  ( -1.000000000000000000, 0.000000000000000000, 0.000000000000000000 ) ) ;
#5407 = LINE ( 'NONE', #5954, #6044 ) ;
#5408 = SURFACE_STYLE_FILL_AREA ( #6113 ) ;
#5409 = CARTESIAN_POINT ( 'NONE',  ( 10.00000000000000000, 42.00000000000000000, 10.00000000000000000 ) ) ;
#5410 = VECTOR ( 'NONE', #1716, 1000.000000000000000 ) ;
#5411 = EDGE_LOOP ( 'NONE', ( #2546, #867, #4311, #2647 ) ) ;
#5412 = ORIENTED_EDGE ( 'NONE', *, *, #354, .F. ) ;
#5413 = AXIS2_PLACEMENT_3D ( 'NONE', #7139, #4174, #2342 ) ;
#5414 = CARTESIAN_POINT ( 'NONE',  ( -73.76644452187068168, 49.96174644486002592, 0.000000000000000000 ) ) ;
#5415 = CARTESIAN_POINT ( 'NONE',  ( 0.000000000000000000, 0.000000000000000000, 2.573333333332999739 ) ) ;
#5416 = CARTESIAN_POINT ( 'NONE',  ( 0.000000000000000000, 0.000000000000000000, -119.9999999999999716 ) ) ;
#5417 = ORIENTED_EDGE ( 'NONE', *, *, #4120, .T. ) ;
#5418 = AXIS2_PLACEMENT_3D ( 'NONE', #4008, #3863, #7518 ) ;
#5419 = VERTEX_POINT ( 'NONE', #6745 ) ;
#5420 = PRODUCT_DEFINITION_SHAPE ( 'NONE', 'NONE',  #7771 ) ;
#5421 = CARTESIAN_POINT ( 'NONE',  ( 207.8429183184021269, 119.9981648402868331, -50.00000000000000000 ) ) ;
#5422 = DIRECTION ( 'NONE',  ( -0.4999999999999918954, -0.8660254037844432595, 0.000000000000000000 ) ) ;
#5423 = CARTESIAN_POINT ( 'NONE',  ( -37.49999999999997868, 0.000000000000000000, -119.9999999999999858 ) ) ;
#5424 = CARTESIAN_POINT ( 'NONE',  ( 2.718977167127998307, 29.87653198021212475, 10.00000000000000000 ) ) ;
#5425 = LINE ( 'NONE', #1767, #2559 ) ;
#5426 = VERTEX_POINT ( 'NONE', #4886 ) ;
#5427 = EDGE_CURVE ( 'NONE', #5633, #3881, #1217, .T. ) ;
#5428 = CARTESIAN_POINT ( 'NONE',  ( 0.000000000000000000, 42.00000000000000000, 10.00000000000000000 ) ) ;
#5429 = LINE ( 'NONE', #1514, #6536 ) ;
#5430 = CARTESIAN_POINT ( 'NONE',  ( 5.250000000000002665, 239.9963296805737230, 10.00000000000000178 ) ) ;
#5431 = DIRECTION ( 'NONE',  ( 0.000000000000000000, 0.000000000000000000, 1.000000000000000000 ) ) ;
#5432 = CIRCLE ( 'NONE', #2039, 6.099504629071904382 ) ;
#5433 = LINE ( 'NONE', #3735, #303 ) ;
#5434 = DIRECTION ( 'NONE',  ( -0.000000000000000000, -0.000000000000000000, 1.000000000000000000 ) ) ;
#5435 = CARTESIAN_POINT ( 'NONE',  ( 125.2481648402868615, 207.8429183184021269, -8.673617379884035472E-15 ) ) ;
#5436 = EDGE_CURVE ( 'NONE', #256, #1325, #7259, .T. ) ;
#5437 = VERTEX_POINT ( 'NONE', #6789 ) ;
#5438 = ORIENTED_EDGE ( 'NONE', *, *, #7451, .T. ) ;
#5439 = EDGE_CURVE ( 'NONE', #544, #3392, #2496, .T. ) ;
#5440 = ORIENTED_EDGE ( 'NONE', *, *, #315, .T. ) ;
#5441 = CARTESIAN_POINT ( 'NONE',  ( 0.000000000000000000, 0.000000000000000000, 0.000000000000000000 ) ) ;
#5442 = CARTESIAN_POINT ( 'NONE',  ( 29.99999999999999289, 0.000000000000000000, -139.9999999999999716 ) ) ;
#5443 = ADVANCED_FACE ( 'NONE', ( #5479 ), #3119, .T. ) ;
#5444 = ORIENTED_EDGE ( 'NONE', *, *, #6878, .F. ) ;
#5445 = ORIENTED_EDGE ( 'NONE', *, *, #2259, .F. ) ;
#5446 = EDGE_CURVE ( 'NONE', #2154, #3231, #7230, .T. ) ;
#5447 = CIRCLE ( 'NONE', #2056, 30.00000000000000000 ) ;
#5448 = DIRECTION ( 'NONE',  ( 1.000000000000000000, 0.000000000000000000, 0.000000000000000000 ) ) ;
#5449 = DIRECTION ( 'NONE',  ( -0.000000000000000000, -0.000000000000000000, -1.000000000000000000 ) ) ;
#5450 = DIRECTION ( 'NONE',  ( -0.000000000000000000, -0.000000000000000000, 1.000000000000000000 ) ) ;
#5451 = AXIS2_PLACEMENT_3D ( 'NONE', #2846, #5164, #2182 ) ;
#5452 = ORIENTED_EDGE ( 'NONE', *, *, #4512, .T. ) ;
#5453 = ORIENTED_EDGE ( 'NONE', *, *, #7454, .T. ) ;
#5454 = VERTEX_POINT ( 'NONE', #6630 ) ;
#5455 = LINE ( 'NONE', #6645, #1213 ) ;
#5456 = DIRECTION ( 'NONE',  ( 1.000000000000000000, 0.000000000000000000, 0.000000000000000000 ) ) ;
#5457 = CIRCLE ( 'NONE', #7350, 8.000000000000000000 ) ;
#5458 = FACE_BOUND ( 'NONE', #4139, .T. ) ;
#5459 = CYLINDRICAL_SURFACE ( 'NONE', #1607, 28.49999999999999645 ) ;
#5460 = CONTEXT_DEPENDENT_SHAPE_REPRESENTATION ( #3344, #6814 ) ;
#5461 = CARTESIAN_POINT ( 'NONE',  ( 4.000000000000000000, -33.63777638310832430, -3.000000000000000000 ) ) ;
#5462 = VERTEX_POINT ( 'NONE', #4255 ) ;
#5463 = CIRCLE ( 'NONE', #4069, 29.99999999999999289 ) ;
#5464 = DIRECTION ( 'NONE',  ( 0.000000000000000000, 0.000000000000000000, 1.000000000000000000 ) ) ;
#5465 = FACE_BOUND ( 'NONE', #5908, .T. ) ;
#5466 = DIRECTION ( 'NONE',  ( -0.9878343221690302212, -0.1555099737793451398, 5.550004789056644515E-17 ) ) ;
#5467 = DIRECTION ( 'NONE',  ( 0.6497489119555339698, -0.7601489008165438488, 0.000000000000000000 ) ) ;
#5468 = AXIS2_PLACEMENT_3D ( 'NONE', #821, #7560, #4409 ) ;
#5469 = DIRECTION ( 'NONE',  ( 1.000000000000000000, 0.000000000000000000, 0.000000000000000000 ) ) ;
#5470 = FACE_OUTER_BOUND ( 'NONE', #4079, .T. ) ;
#5471 = ORIENTED_EDGE ( 'NONE', *, *, #316, .F. ) ;
#5472 = ORIENTED_EDGE ( 'NONE', *, *, #5916, .T. ) ;
#5473 = EDGE_CURVE ( 'NONE', #3642, #7134, #1945, .T. ) ;
#5474 = ORIENTED_EDGE ( 'NONE', *, *, #263, .F. ) ;
#5475 = CYLINDRICAL_SURFACE ( 'NONE', #889, 40.00000000000000711 ) ;
#5476 = CARTESIAN_POINT ( 'NONE',  ( 0.000000000000000000, 0.000000000000000000, -4.149444346342716194 ) ) ;
#5477 = EDGE_CURVE ( 'NONE', #699, #294, #3328, .T. ) ;
#5478 = EDGE_CURVE ( 'NONE', #3350, #2919, #7362, .T. ) ;
#5479 = FACE_OUTER_BOUND ( 'NONE', #5567, .T. ) ;
#5480 = AXIS2_PLACEMENT_3D ( 'NONE', #3101, #4199, #575 ) ;
#5481 = EDGE_CURVE ( 'NONE', #4724, #4160, #6473, .T. ) ;
#5482 = PRODUCT_DEFINITION_SHAPE ( 'NONE', 'NONE',  #7796 ) ;
#5483 = ORIENTED_EDGE ( 'NONE', *, *, #3406, .F. ) ;
#5484 = ORIENTED_EDGE ( 'NONE', *, *, #3173, .F. ) ;
#5485 = DIRECTION ( 'NONE',  ( 0.000000000000000000, 0.000000000000000000, -1.000000000000000000 ) ) ;
#5486 = EDGE_CURVE ( 'NONE', #4741, #5275, #7408, .T. ) ;
#5487 = CARTESIAN_POINT ( 'NONE',  ( -10.00000000000000000, 42.00000000000000000, 0.000000000000000000 ) ) ;
#5488 = PRESENTATION_LAYER_ASSIGNMENT (  '', '', ( #2978 ) ) ;
#5489 = CARTESIAN_POINT ( 'NONE',  ( -30.00000000000000000, 3.673940397442059178E-15, 10.00000000000000000 ) ) ;
#5490 = ORIENTED_EDGE ( 'NONE', *, *, #2992, .F. ) ;
#5491 = VERTEX_POINT ( 'NONE', #4489 ) ;
#5492 = TOROIDAL_SURFACE ( 'NONE', #4991, 33.75000000000000000, 2.250000000000000444 ) ;
#5493 = CARTESIAN_POINT ( 'NONE',  ( -68.76644452187068168, 49.96174644486002592, -40.00000000000000000 ) ) ;
#5494 = DIRECTION ( 'NONE',  ( 1.000000000000000000, 0.000000000000000000, 0.000000000000000000 ) ) ;
#5495 = CARTESIAN_POINT ( 'NONE',  ( -32.81578194438969120, 1.484218055610309728, -3.000000000000000000 ) ) ;
#5496 = CARTESIAN_POINT ( 'NONE',  ( -0.7500000000000000000, -37.49249924984995630, 0.000000000000000000 ) ) ;
#5497 = CARTESIAN_POINT ( 'NONE',  ( -29.99999999999999289, 3.673940397442058389E-15, -60.00000000000000000 ) ) ;
#5498 = ORIENTED_EDGE ( 'NONE', *, *, #3653, .T. ) ;
#5499 = VECTOR ( 'NONE', #395, 1000.000000000000000 ) ;
#5500 = DIRECTION ( 'NONE',  ( -0.000000000000000000, 0.000000000000000000, 1.000000000000000000 ) ) ;
#5501 = CIRCLE ( 'NONE', #7141, 37.19999999999999574 ) ;
#5502 = CARTESIAN_POINT ( 'NONE',  ( 0.000000000000000000, 0.000000000000000000, -60.00000000000000711 ) ) ;
#5503 = DIRECTION ( 'NONE',  ( 1.000000000000000000, 0.000000000000000000, 0.000000000000000000 ) ) ;
#5504 = DIRECTION ( 'NONE',  ( 0.7601489008165417394, 0.6497489119555366344, 1.931932416011734352E-18 ) ) ;
#5505 = APPLICATION_CONTEXT ( 'automotive_design' ) ;
#5506 = DIRECTION ( 'NONE',  ( 0.000000000000000000, 0.000000000000000000, 1.000000000000000000 ) ) ;
#5507 = DIRECTION ( 'NONE',  ( -0.000000000000000000, -0.000000000000000000, 1.000000000000000000 ) ) ;
#5508 = LINE ( 'NONE', #4097, #5582 ) ;
#5509 = ORIENTED_EDGE ( 'NONE', *, *, #6297, .T. ) ;
#5510 = AXIS2_PLACEMENT_3D ( 'NONE', #287, #845, #368 ) ;
#5511 = VERTEX_POINT ( 'NONE', #3825 ) ;
#5512 = UNCERTAINTY_MEASURE_WITH_UNIT (LENGTH_MEASURE( 1.000000000000000082E-05 ), #4614, 'distance_accuracy_value', 'NONE');
#5513 = ORIENTED_EDGE ( 'NONE', *, *, #3266, .T. ) ;
#5514 = CARTESIAN_POINT ( 'NONE',  ( 10.16320117273318679, -26.62629042736811869, -119.9999999999999716 ) ) ;
#5515 = CIRCLE ( 'NONE', #3995, 32.81578194438969120 ) ;
#5516 = DIRECTION ( 'NONE',  ( 0.000000000000000000, 0.000000000000000000, 1.000000000000000000 ) ) ;
#5517 = VERTEX_POINT ( 'NONE', #2759 ) ;
#5518 = ORIENTED_EDGE ( 'NONE', *, *, #312, .T. ) ;
#5519 = ORIENTED_EDGE ( 'NONE', *, *, #2685, .F. ) ;
#5520 = AXIS2_PLACEMENT_3D ( 'NONE', #6839, #6285, #6916 ) ;
#5521 = EDGE_CURVE ( 'NONE', #3378, #6651, #5155, .T. ) ;
#5522 = CYLINDRICAL_SURFACE ( 'NONE', #4414, 5.250000000000004441 ) ;
#5523 = FILL_AREA_STYLE_COLOUR ( '', #4972 ) ;
#5524 = VECTOR ( 'NONE', #5191, 1000.000000000000000 ) ;
#5525 = FACE_OUTER_BOUND ( 'NONE', #3893, .T. ) ;
#5526 = FACE_OUTER_BOUND ( 'NONE', #7476, .T. ) ;
#5527 = ORIENTED_EDGE ( 'NONE', *, *, #843, .T. ) ;
#5528 = EDGE_CURVE ( 'NONE', #3290, #4712, #3934, .T. ) ;
#5529 = AXIS2_PLACEMENT_3D ( 'NONE', #1459, #3354, #5124 ) ;
#5530 = ORIENTED_EDGE ( 'NONE', *, *, #2729, .T. ) ;
#5531 = DIRECTION ( 'NONE',  ( 5.551115123125782702E-17, -0.000000000000000000, 1.000000000000000000 ) ) ;
#5532 = DIRECTION ( 'NONE',  ( 0.000000000000000000, 0.000000000000000000, -1.000000000000000000 ) ) ;
#5533 = FACE_BOUND ( 'NONE', #7718, .T. ) ;
#5534 = CARTESIAN_POINT ( 'NONE',  ( 0.000000000000000000, 0.000000000000000000, 0.000000000000000000 ) ) ;
#5535 = AXIS2_PLACEMENT_3D ( 'NONE', #3069, #145, #7287 ) ;
#5536 = DIRECTION ( 'NONE',  ( 0.000000000000000000, 0.000000000000000000, -1.000000000000000000 ) ) ;
#5537 = ORIENTED_EDGE ( 'NONE', *, *, #4363, .F. ) ;
#5538 = EDGE_CURVE ( 'NONE', #816, #4399, #2018, .T. ) ;
#5539 = AXIS2_PLACEMENT_3D ( 'NONE', #6423, #3272, #5073 ) ;
#5540 = DIRECTION ( 'NONE',  ( 0.000000000000000000, 0.000000000000000000, 1.000000000000000000 ) ) ;
#5541 = ADVANCED_FACE ( 'NONE', ( #1530 ), #1450, .F. ) ;
#5542 = CARTESIAN_POINT ( 'NONE',  ( 8.000000000000000000, 0.7809653281576058870, -4.700000000000001066 ) ) ;
#5543 = CARTESIAN_POINT ( 'NONE',  ( -0.7500000000000000000, -37.49249924984995630, -3.000000000000000000 ) ) ;
#5544 = APPLICATION_PROTOCOL_DEFINITION ( 'draft international standard', 'automotive_design', 1998, #7169 ) ;
#5545 = PRODUCT_DEFINITION_SHAPE ( 'NONE', 'NONE',  #7781 ) ;
#5546 = CARTESIAN_POINT ( 'NONE',  ( -145.1064334105735725, 38.00161816110971813, 10.00000000000000000 ) ) ;
#5547 = CARTESIAN_POINT ( 'NONE',  ( -119.9981648402875578, 207.8429183184017859, -120.0000000000000000 ) ) ;
#5548 = FACE_BOUND ( 'NONE', #372, .T. ) ;
#5549 = ORIENTED_EDGE ( 'NONE', *, *, #6201, .T. ) ;
#5550 = ORIENTED_EDGE ( 'NONE', *, *, #4424, .T. ) ;
#5551 = ORIENTED_EDGE ( 'NONE', *, *, #672, .T. ) ;
#5552 = AXIS2_PLACEMENT_3D ( 'NONE', #466, #6549, #5914 ) ;
#5553 = DIRECTION ( 'NONE',  ( 0.000000000000000000, 0.000000000000000000, 1.000000000000000000 ) ) ;
#5554 =( NAMED_UNIT ( * ) PLANE_ANGLE_UNIT ( ) SI_UNIT ( $, .RADIAN. ) );
#5555 = FILL_AREA_STYLE ('',( #3306 ) ) ;
#5556 = CARTESIAN_POINT ( 'NONE',  ( -207.8429183184020985, 119.9981648402869467, 10.00000000000000178 ) ) ;
#5557 = ORIENTED_EDGE ( 'NONE', *, *, #2357, .F. ) ;
#5558 = VERTEX_POINT ( 'NONE', #5635 ) ;
#5559 = AXIS2_PLACEMENT_3D ( 'NONE', #24, #1917, #59 ) ;
#5560 = ORIENTED_EDGE ( 'NONE', *, *, #7176, .F. ) ;
#5561 = CARTESIAN_POINT ( 'NONE',  ( 0.000000000000000000, 0.000000000000000000, 10.00000000000000000 ) ) ;
#5562 = SURFACE_STYLE_USAGE ( .BOTH. , #3167 ) ;
#5563 = CARTESIAN_POINT ( 'NONE',  ( 0.000000000000000000, 0.000000000000000000, -139.9999999999999716 ) ) ;
#5564 = DIRECTION ( 'NONE',  ( -0.5000000000000037748, 0.8660254037844364872, 0.000000000000000000 ) ) ;
#5565 = EDGE_LOOP ( 'NONE', ( #1180, #2611, #6994, #4944 ) ) ;
#5566 = AXIS2_PLACEMENT_3D ( 'NONE', #873, #762, #3289 ) ;
#5567 = EDGE_LOOP ( 'NONE', ( #726, #2340, #7242, #5066 ) ) ;
#5568 = EDGE_CURVE ( 'NONE', #6712, #2925, #2824, .T. ) ;
#5569 = FACE_OUTER_BOUND ( 'NONE', #1630, .T. ) ;
#5570 = PLANE ( 'NONE',  #1417 ) ;
#5571 = DIRECTION ( 'NONE',  ( -0.000000000000000000, 0.000000000000000000, -1.000000000000000000 ) ) ;
#5572 = EDGE_CURVE ( 'NONE', #6942, #5886, #7730, .T. ) ;
#5573 = AXIS2_PLACEMENT_3D ( 'NONE', #4778, #2349, #4738 ) ;
#5574 = ADVANCED_FACE ( 'NONE', ( #6232 ), #3348, .T. ) ;
#5575 = UNCERTAINTY_MEASURE_WITH_UNIT (LENGTH_MEASURE( 1.000000000000000082E-05 ), #1673, 'distance_accuracy_value', 'NONE');
#5576 = EDGE_CURVE ( 'NONE', #7389, #7629, #1715, .T. ) ;
#5577 = CARTESIAN_POINT ( 'NONE',  ( 0.000000000000000000, 0.000000000000000000, -4.149444346342716194 ) ) ;
#5578 = EDGE_LOOP ( 'NONE', ( #7095, #2751 ) ) ;
#5579 = ADVANCED_FACE ( 'NONE', ( #7446 ), #6862, .T. ) ;
#5580 = B_SPLINE_CURVE_WITH_KNOTS ( 'NONE', 3,
 ( #5331, #5170, #2268, #1022, #5884, #7573 ),
 .UNSPECIFIED., .F., .F.,
 ( 4, 2, 4 ),
 ( 2.380731629562773498E-07, 0.002336973833157560305, 0.004673709593152164388 ),
 .UNSPECIFIED. ) ;
#5581 = PLANE ( 'NONE',  #714 ) ;
#5582 = VECTOR ( 'NONE', #1924, 1000.000000000000000 ) ;
#5583 = LINE ( 'NONE', #2703, #6883 ) ;
#5584 = EDGE_CURVE ( 'NONE', #3312, #6072, #1307, .T. ) ;
#5585 = LINE ( 'NONE', #5622, #614 ) ;
#5586 = CARTESIAN_POINT ( 'NONE',  ( 10.00000000000000000, 0.000000000000000000, 0.000000000000000000 ) ) ;
#5587 = PRODUCT_CONTEXT ( 'NONE', #1220, 'mechanical' ) ;
#5588 = CARTESIAN_POINT ( 'NONE',  ( 0.000000000000000000, 0.000000000000000000, -119.9999999999999716 ) ) ;
#5589 = CARTESIAN_POINT ( 'NONE',  ( -20.63749999999999574, 4.316879966994420283E-15, 35.25000000000000000 ) ) ;
#5590 = CIRCLE ( 'NONE', #4703, 5.250000000000000888 ) ;
#5591 = ORIENTED_EDGE ( 'NONE', *, *, #5338, .T. ) ;
#5592 = ORIENTED_EDGE ( 'NONE', *, *, #7459, .F. ) ;
#5593 = ORIENTED_EDGE ( 'NONE', *, *, #3837, .T. ) ;
#5594 = CIRCLE ( 'NONE', #4584, 28.50000000000000711 ) ;
#5595 = VECTOR ( 'NONE', #1910, 1000.000000000000000 ) ;
#5596 = DIRECTION ( 'NONE',  ( 1.000000000000000000, 0.000000000000000000, 0.000000000000000000 ) ) ;
#5597 =( LENGTH_UNIT ( ) NAMED_UNIT ( * ) SI_UNIT ( .MILLI., .METRE. ) );
#5598 = DIRECTION ( 'NONE',  ( 1.000000000000000000, 0.000000000000000000, 0.000000000000000000 ) ) ;
#5599 = CIRCLE ( 'NONE', #2966, 28.50000000000000711 ) ;
#5600 = ORIENTED_EDGE ( 'NONE', *, *, #668, .T. ) ;
#5601 = VECTOR ( 'NONE', #674, 999.9999999999998863 ) ;
#5602 = ORIENTED_EDGE ( 'NONE', *, *, #4653, .F. ) ;
#5603 = CARTESIAN_POINT ( 'NONE',  ( -64.59444452187068464, 49.96174644486002592, 25.00000000000000000 ) ) ;
#5605 = MECHANICAL_DESIGN_GEOMETRIC_PRESENTATION_REPRESENTATION (  '', ( #3836 ), #6739 ) ;
#5604 =( NAMED_UNIT ( * ) SI_UNIT ( $, .STERADIAN. ) SOLID_ANGLE_UNIT ( ) );
#5606 = PRESENTATION_LAYER_ASSIGNMENT (  '', '', ( #1577 ) ) ;
#5607 = FACE_OUTER_BOUND ( 'NONE', #4498, .T. ) ;
#5608 = DIRECTION ( 'NONE',  ( -0.000000000000000000, -0.000000000000000000, 1.000000000000000000 ) ) ;
#5609 = VERTEX_POINT ( 'NONE', #5003 ) ;
#5610 = AXIS2_PLACEMENT_3D ( 'NONE', #1775, #3033, #4206 ) ;
#5611 = PRODUCT_DEFINITION_SHAPE ( 'NONE', 'NONE',  #7791 ) ;
#5612 = CARTESIAN_POINT ( 'NONE',  ( -1.734723475976807094E-15, 9.237604307034017026, -0.7145311798163319628 ) ) ;
#5613 = CARTESIAN_POINT ( 'NONE',  ( -68.76644452187024115, -49.96174644486060856, 10.00000000000000000 ) ) ;
#5614 = FACE_OUTER_BOUND ( 'NONE', #4664, .T. ) ;
#5615 = DIRECTION ( 'NONE',  ( -1.000000000000000000, 0.000000000000000000, 0.000000000000000000 ) ) ;
#5616 = ORIENTED_EDGE ( 'NONE', *, *, #2068, .F. ) ;
#5617 = ADVANCED_FACE ( 'NONE', ( #4565 ), #5706, .F. ) ;
#5618 = AXIS2_PLACEMENT_3D ( 'NONE', #2321, #4239, #2406 ) ;
#5619 = DIRECTION ( 'NONE',  ( 0.000000000000000000, 0.000000000000000000, -1.000000000000000000 ) ) ;
#5620 = FACE_OUTER_BOUND ( 'NONE', #6386, .T. ) ;
#5621 = EDGE_CURVE ( 'NONE', #7346, #1373, #5670, .T. ) ;
#5622 = CARTESIAN_POINT ( 'NONE',  ( 39.64284999284934941, -144.6666666666667140, 5.000000000000000000 ) ) ;
#5623 = LINE ( 'NONE', #2630, #6773 ) ;
#5624 =( NAMED_UNIT ( * ) PLANE_ANGLE_UNIT ( ) SI_UNIT ( $, .RADIAN. ) );
#5625 = CIRCLE ( 'NONE', #2236, 30.30000000000000071 ) ;
#5626 = CARTESIAN_POINT ( 'NONE',  ( 1.469553684752138043E-14, 239.9963296805737230, -8.673617379884035472E-15 ) ) ;
#5627 = DIRECTION ( 'NONE',  ( 1.000000000000000000, 0.000000000000000000, 0.000000000000000000 ) ) ;
#5628 = EDGE_LOOP ( 'NONE', ( #2671, #6327 ) ) ;
#5629 = ORIENTED_EDGE ( 'NONE', *, *, #3837, .F. ) ;
#5630 = ORIENTED_EDGE ( 'NONE', *, *, #6305, .F. ) ;
#5631 = EDGE_CURVE ( 'NONE', #7368, #5239, #5594, .T. ) ;
#5632 = AXIS2_PLACEMENT_3D ( 'NONE', #4734, #6556, #5965 ) ;
#5633 = VERTEX_POINT ( 'NONE', #5117 ) ;
#5634 = CARTESIAN_POINT ( 'NONE',  ( -58.76644452187068168, 49.96174644486002592, -40.00000000000000000 ) ) ;
#5635 = CARTESIAN_POINT ( 'NONE',  ( -105.4635834177243794, 106.6650485055563990, 10.00000000000000000 ) ) ;
#5636 = ORIENTED_EDGE ( 'NONE', *, *, #4620, .T. ) ;
#5637 = VERTEX_POINT ( 'NONE', #4528 ) ;
#5638 = CIRCLE ( 'NONE', #2254, 5.249999999999976907 ) ;
#5639 = DIRECTION ( 'NONE',  ( -0.000000000000000000, -0.000000000000000000, -1.000000000000000000 ) ) ;
#5640 = EDGE_CURVE ( 'NONE', #7689, #1722, #5084, .T. ) ;
#5641 = SURFACE_SIDE_STYLE ('',( #1498 ) ) ;
#5642 = DIRECTION ( 'NONE',  ( -0.000000000000000000, -0.000000000000000000, -1.000000000000000000 ) ) ;
#5643 = CARTESIAN_POINT ( 'NONE',  ( 3.200000000000008171, 0.000000000000000000, -30.00000000000000000 ) ) ;
#5644 = VERTEX_POINT ( 'NONE', #5946 ) ;
#5645 = VECTOR ( 'NONE', #3717, 1000.000000000000114 ) ;
#5646 = VECTOR ( 'NONE', #1366, 1000.000000000000000 ) ;
#5647 = CARTESIAN_POINT ( 'NONE',  ( -1.310872448937997925, 8.480771745766398695, -0.3173508448886566136 ) ) ;
#5648 = CARTESIAN_POINT ( 'NONE',  ( 0.000000000000000000, 0.000000000000000000, 10.00000000000000000 ) ) ;
#5649 = DIRECTION ( 'NONE',  ( -0.000000000000000000, -0.000000000000000000, 1.000000000000000000 ) ) ;
#5650 = DIRECTION ( 'NONE',  ( -3.081487911019577365E-33, 2.775557561562891967E-17, 1.000000000000000000 ) ) ;
#5651 = EDGE_LOOP ( 'NONE', ( #3892, #172, #2682, #5118 ) ) ;
#5652 = AXIS2_PLACEMENT_3D ( 'NONE', #1578, #5162, #3870 ) ;
#5653 = CARTESIAN_POINT ( 'NONE',  ( 125.2481648402866341, 207.8429183184022122, -50.00000000000000000 ) ) ;
#5654 = CARTESIAN_POINT ( 'NONE',  ( 0.000000000000000000, 0.000000000000000000, -3.000000000000000000 ) ) ;
#5655 = CIRCLE ( 'NONE', #4148, 40.00000000000000711 ) ;
#5656 = ADVANCED_FACE ( 'NONE', ( #5235 ), #1694, .T. ) ;
#5657 = DIRECTION ( 'NONE',  ( -1.000000000000000000, 0.000000000000000000, 0.000000000000000000 ) ) ;
#5658 = FACE_OUTER_BOUND ( 'NONE', #2350, .T. ) ;
#5659 = APPLICATION_PROTOCOL_DEFINITION ( 'draft international standard', 'automotive_design', 1998, #5505 ) ;
#5660 = CARTESIAN_POINT ( 'NONE',  ( 0.000000000000000000, 0.000000000000000000, -119.9999999999999858 ) ) ;
#5661 = VERTEX_POINT ( 'NONE', #1689 ) ;
#5662 = EDGE_LOOP ( 'NONE', ( #6350, #626, #2048, #3017 ) ) ;
#5663 = VECTOR ( 'NONE', #5667, 1000.000000000000000 ) ;
#5664 = VERTEX_POINT ( 'NONE', #7051 ) ;
#5665 = VERTEX_POINT ( 'NONE', #2873 ) ;
#5666 = DIRECTION ( 'NONE',  ( 0.000000000000000000, 0.000000000000000000, -1.000000000000000000 ) ) ;
#5667 = DIRECTION ( 'NONE',  ( -0.000000000000000000, -0.000000000000000000, -1.000000000000000000 ) ) ;
#5668 =( NAMED_UNIT ( * ) PLANE_ANGLE_UNIT ( ) SI_UNIT ( $, .RADIAN. ) );
#5669 = AXIS2_PLACEMENT_3D ( 'NONE', #5122, #5046, #3829 ) ;
#5670 = LINE ( 'NONE', #2677, #7479 ) ;
#5671 = ADVANCED_FACE ( 'NONE', ( #1735 ), #1648, .T. ) ;
#5672 = PRODUCT ( 'Guide Rail Bracket', 'Guide Rail Bracket', '', ( #6889 ) ) ;
#5673 = ORIENTED_EDGE ( 'NONE', *, *, #512, .T. ) ;
#5674 = ADVANCED_FACE ( 'NONE', ( #7088 ), #4088, .T. ) ;
#5675 = ORIENTED_EDGE ( 'NONE', *, *, #897, .T. ) ;
#5676 = MANIFOLD_SOLID_BREP ( 'Cavity1', #1446 ) ;
#5677 = CARTESIAN_POINT ( 'NONE',  ( -68.76644452187072432, 49.96174644486006855, -40.00000000000000000 ) ) ;
#5678 = EDGE_CURVE ( 'NONE', #3132, #7232, #1949, .T. ) ;
#5679 = DIRECTION ( 'NONE',  ( -1.000000000000000000, 0.000000000000000000, 0.000000000000000000 ) ) ;
#5680 = LINE ( 'NONE', #270, #6159 ) ;
#5681 = AXIS2_PLACEMENT_3D ( 'NONE', #2014, #5072, #7480 ) ;
#5682 = CYLINDRICAL_SURFACE ( 'NONE', #4692, 28.50000000000000711 ) ;
#5683 = ORIENTED_EDGE ( 'NONE', *, *, #7357, .T. ) ;
#5684 = ADVANCED_FACE ( 'NONE', ( #5194 ), #5358, .T. ) ;
#5685 = CARTESIAN_POINT ( 'NONE',  ( 0.000000000000000000, 0.000000000000000000, -119.9999999999999858 ) ) ;
#5686 = DIRECTION ( 'NONE',  ( 1.000000000000000000, 0.000000000000000000, 0.000000000000000000 ) ) ;
#5687 = LINE ( 'NONE', #1468, #4383 ) ;
#5688 = CARTESIAN_POINT ( 'NONE',  ( 8.000000000000000000, -4.618802153517011178, -3.985468820183668104 ) ) ;
#5689 = ORIENTED_EDGE ( 'NONE', *, *, #2415, .F. ) ;
#5690 = DIRECTION ( 'NONE',  ( 1.000000000000000000, 0.000000000000000000, 0.000000000000000000 ) ) ;
#5691 = AXIS2_PLACEMENT_3D ( 'NONE', #1665, #321, #2775 ) ;
#5692 = LINE ( 'NONE', #2276, #681 ) ;
#5693 = DIRECTION ( 'NONE',  ( -1.000000000000000000, 0.000000000000000000, 0.000000000000000000 ) ) ;
#5694 = FACE_OUTER_BOUND ( 'NONE', #2926, .T. ) ;
#5695 = SHAPE_DEFINITION_REPRESENTATION ( #3593, #637 ) ;
#5696 = ORIENTED_EDGE ( 'NONE', *, *, #3269, .T. ) ;
#5697 = ORIENTED_EDGE ( 'NONE', *, *, #6639, .T. ) ;
#5698 = ORIENTED_EDGE ( 'NONE', *, *, #1820, .F. ) ;
#5699 = AXIS2_PLACEMENT_3D ( 'NONE', #3909, #4055, #5758 ) ;
#5700 = AXIS2_PLACEMENT_3D ( 'NONE', #723, #6093, #2552 ) ;
#5701 = EDGE_LOOP ( 'NONE', ( #5390, #7005, #109, #5630 ) ) ;
#5702 = CARTESIAN_POINT ( 'NONE',  ( 0.000000000000000000, 0.000000000000000000, -50.00000000000000000 ) ) ;
#5703 = DIRECTION ( 'NONE',  ( 1.000000000000000000, 0.000000000000000000, -0.000000000000000000 ) ) ;
#5704 = CARTESIAN_POINT ( 'NONE',  ( 0.000000000000000000, 0.000000000000000000, 0.000000000000000000 ) ) ;
#5705 = CIRCLE ( 'NONE', #3196, 30.00000000000000000 ) ;
#5706 = PLANE ( 'NONE',  #2462 ) ;
#5707 = EDGE_LOOP ( 'NONE', ( #5316, #5779, #5689, #6389 ) ) ;
#5708 = ADVANCED_FACE ( 'NONE', ( #2373 ), #7170, .T. ) ;
#5709 = EDGE_LOOP ( 'NONE', ( #1856, #3162, #130, #884 ) ) ;
#5710 = AXIS2_PLACEMENT_3D ( 'NONE', #6040, #1296, #2573 ) ;
#5711 = EDGE_LOOP ( 'NONE', ( #698, #1328, #5158, #2636 ) ) ;
#5712 = ADVANCED_FACE ( 'NONE', ( #1776 ), #3450, .T. ) ;
#5713 = EDGE_CURVE ( 'NONE', #7510, #5243, #4207, .T. ) ;
#5714 = CARTESIAN_POINT ( 'NONE',  ( -11.50644898236017433, -35.69105814929478981, 0.000000000000000000 ) ) ;
#5715 = EDGE_CURVE ( 'NONE', #1947, #6615, #5906, .T. ) ;
#5716 = FACE_OUTER_BOUND ( 'NONE', #4220, .T. ) ;
#5717 = VECTOR ( 'NONE', #2173, 1000.000000000000000 ) ;
#5718 = CIRCLE ( 'NONE', #7731, 5.000000000000004441 ) ;
#5719 = CARTESIAN_POINT ( 'NONE',  ( -5.250000000000509814, 239.9963296805737230, -50.00000000000000000 ) ) ;
#5720 = ORIENTED_EDGE ( 'NONE', *, *, #3129, .F. ) ;
#5721 = ADVANCED_FACE ( 'NONE', ( #2836 ), #3204, .T. ) ;
#5722 = CIRCLE ( 'NONE', #2085, 29.99999999999999289 ) ;
#5723 = DIRECTION ( 'NONE',  ( 0.000000000000000000, 0.000000000000000000, 1.000000000000000000 ) ) ;
#5724 = CARTESIAN_POINT ( 'NONE',  ( -37.49999999999997868, 0.000000000000000000, -112.9999999999999716 ) ) ;
#5725 = CARTESIAN_POINT ( 'NONE',  ( 29.99999999999999289, 2.565854121688507820E-48, -122.9999999999999716 ) ) ;
#5726 = MANIFOLD_SOLID_BREP ( 'M10 Clearance Hole1', #6748 ) ;
#5727 = DIRECTION ( 'NONE',  ( 0.000000000000000000, 0.000000000000000000, 1.000000000000000000 ) ) ;
#5728 = ORIENTED_EDGE ( 'NONE', *, *, #3850, .F. ) ;
#5729 = MECHANICAL_DESIGN_GEOMETRIC_PRESENTATION_REPRESENTATION (  '', ( #6867 ), #7745 ) ;
#5730 = CYLINDRICAL_SURFACE ( 'NONE', #959, 5.250000000000004441 ) ;
#5731 = DIRECTION ( 'NONE',  ( 1.224646799147353207E-16, 1.000000000000000000, 0.000000000000000000 ) ) ;
#5732 = DIRECTION ( 'NONE',  ( -1.000000000000000000, 0.000000000000000000, 0.000000000000000000 ) ) ;
#5733 = AXIS2_PLACEMENT_3D ( 'NONE', #579, #2205, #2869 ) ;
#5734 = DIRECTION ( 'NONE',  ( -0.000000000000000000, -0.000000000000000000, -1.000000000000000000 ) ) ;
#5735 = CARTESIAN_POINT ( 'NONE',  ( -4.000000000000004441, -6.928203230275506108, 0.000000000000000000 ) ) ;
#5736 = CONTEXT_DEPENDENT_SHAPE_REPRESENTATION ( #7669, #6872 ) ;
#5737 = LINE ( 'NONE', #6184, #564 ) ;
#5738 = ORIENTED_EDGE ( 'NONE', *, *, #2037, .F. ) ;
#5739 = PRESENTATION_LAYER_ASSIGNMENT (  '', '', ( #3729 ) ) ;
#5740 = ORIENTED_EDGE ( 'NONE', *, *, #4278, .T. ) ;
#5741 = MANIFOLD_SOLID_BREP ( 'OuterRace', #4474 ) ;
#5742 = VERTEX_POINT ( 'NONE', #732 ) ;
#5743 = CARTESIAN_POINT ( 'NONE',  ( 1.677050983124841466, 0.000000000000000000, 0.000000000000000000 ) ) ;
#5744 = CARTESIAN_POINT ( 'NONE',  ( -4.000000000000000000, -33.63777638310832430, -3.000000000000000000 ) ) ;
#5745 = CIRCLE ( 'NONE', #1591, 28.50000000000000355 ) ;
#5746 = DIRECTION ( 'NONE',  ( -0.000000000000000000, -0.000000000000000000, 1.000000000000000000 ) ) ;
#5747 = CARTESIAN_POINT ( 'NONE',  ( 0.000000000000000000, 0.000000000000000000, -4.700000000000000178 ) ) ;
#5748 = CARTESIAN_POINT ( 'NONE',  ( 0.000000000000000000, 0.000000000000000000, 0.000000000000000000 ) ) ;
#5749 = DIRECTION ( 'NONE',  ( -0.000000000000000000, -0.000000000000000000, -1.000000000000000000 ) ) ;
#5750 = ORIENTED_EDGE ( 'NONE', *, *, #7701, .F. ) ;
#5751 = VECTOR ( 'NONE', #5259, 1000.000000000000000 ) ;
#5752 = VERTEX_POINT ( 'NONE', #6622 ) ;
#5753 = ORIENTED_EDGE ( 'NONE', *, *, #3745, .F. ) ;
#5754 = B_SPLINE_CURVE_WITH_KNOTS ( 'NONE', 3,
 ( #5220, #7072, #2192, #2273, #7621, #485, #1670, #6996 ),
 .UNSPECIFIED., .F., .F.,
 ( 4, 2, 2, 4 ),
 ( 0.004673709593152171327, 0.005837709341827658147, 0.007001709090503144967, 0.009329708587854113402 ),
 .UNSPECIFIED. ) ;
#5755 = FACE_OUTER_BOUND ( 'NONE', #3143, .T. ) ;
#5756 = AXIS2_PLACEMENT_3D ( 'NONE', #2083, #212, #1478 ) ;
#5757 = CARTESIAN_POINT ( 'NONE',  ( -68.76644452187068168, 49.96174644486002592, 24.17200000000001125 ) ) ;
#5758 = DIRECTION ( 'NONE',  ( 1.000000000000000000, 0.000000000000000000, 0.000000000000000000 ) ) ;
#5759 = ORIENTED_EDGE ( 'NONE', *, *, #125, .F. ) ;
#5760 = CIRCLE ( 'NONE', #5700, 1.286666666666999914 ) ;
#5761 = EDGE_CURVE ( 'NONE', #3153, #6982, #7364, .T. ) ;
#5762 = CARTESIAN_POINT ( 'NONE',  ( -279.9963296805736945, 3.428966089163216048E-14, 576.0908266162076643 ) ) ;
#5763 = DIRECTION ( 'NONE',  ( 1.000000000000000000, 0.000000000000000000, -0.000000000000000000 ) ) ;
#5764 = DIRECTION ( 'NONE',  ( -0.000000000000000000, -0.000000000000000000, 1.000000000000000000 ) ) ;
#5765 = DIRECTION ( 'NONE',  ( -0.000000000000000000, -0.000000000000000000, 1.000000000000000000 ) ) ;
#5766 = EDGE_CURVE ( 'NONE', #1095, #2423, #2708, .T. ) ;
#5767 = ORIENTED_EDGE ( 'NONE', *, *, #6977, .F. ) ;
#5768 = SHAPE_REPRESENTATION ( 'Guide Rail Bracket', ( #7485 ), #7608 ) ;
#5769 = EDGE_CURVE ( 'NONE', #2049, #1972, #5433, .T. ) ;
#5770 = CYLINDRICAL_SURFACE ( 'NONE', #7013, 8.000000000000000000 ) ;
#5771 = SURFACE_STYLE_FILL_AREA ( #4744 ) ;
#5772 = DIRECTION ( 'NONE',  ( -0.000000000000000000, -0.000000000000000000, 1.000000000000000000 ) ) ;
#5773 = DIRECTION ( 'NONE',  ( 0.000000000000000000, -1.224646799147352961E-16, 1.000000000000000000 ) ) ;
#5774 = DIRECTION ( 'NONE',  ( -0.000000000000000000, -0.000000000000000000, 1.000000000000000000 ) ) ;
#5775 = CONTEXT_DEPENDENT_SHAPE_REPRESENTATION ( #363, #3163 ) ;
#5776 = VECTOR ( 'NONE', #1477, 1000.000000000000000 ) ;
#5777 = EDGE_CURVE ( 'NONE', #3595, #1611, #6143, .T. ) ;
#5778 = CARTESIAN_POINT ( 'NONE',  ( -30.00000000000000000, 3.673940397442059178E-15, 0.000000000000000000 ) ) ;
#5779 = ORIENTED_EDGE ( 'NONE', *, *, #991, .F. ) ;
#5780 = EDGE_LOOP ( 'NONE', ( #5324, #5015, #4821, #265 ) ) ;
#5781 = EDGE_LOOP ( 'NONE', ( #7177, #2133, #1669 ) ) ;
#5782 = EDGE_CURVE ( 'NONE', #6148, #6492, #6103, .T. ) ;
#5783 = VECTOR ( 'NONE', #5384, 1000.000000000000000 ) ;
#5784 = ORIENTED_EDGE ( 'NONE', *, *, #6496, .F. ) ;
#5785 = DIRECTION ( 'NONE',  ( 1.000000000000000000, 0.000000000000000000, 0.000000000000000000 ) ) ;
#5786 = DIRECTION ( 'NONE',  ( 1.000000000000000000, 0.000000000000000000, 0.000000000000000000 ) ) ;
#5787 = CARTESIAN_POINT ( 'NONE',  ( 0.000000000000000000, 0.000000000000000000, -50.00000000000004263 ) ) ;
#5788 = CARTESIAN_POINT ( 'NONE',  ( -68.76644452187068168, 49.96174644486002592, -54.70000000000000284 ) ) ;
#5789 = DIRECTION ( 'NONE',  ( -0.000000000000000000, -0.000000000000000000, -1.000000000000000000 ) ) ;
#5790 = CIRCLE ( 'NONE', #5156, 5.250000000000004441 ) ;
#5791 = VERTEX_POINT ( 'NONE', #5546 ) ;
#5792 = ORIENTED_EDGE ( 'NONE', *, *, #4020, .T. ) ;
#5793 = ORIENTED_EDGE ( 'NONE', *, *, #1621, .T. ) ;
#5794 = CIRCLE ( 'NONE', #2030, 28.50000000000000711 ) ;
#5795 = DIRECTION ( 'NONE',  ( 1.000000000000000000, 0.000000000000000000, 0.000000000000000000 ) ) ;
#5796 =( LENGTH_UNIT ( ) NAMED_UNIT ( * ) SI_UNIT ( .MILLI., .METRE. ) );
#5797 = DIRECTION ( 'NONE',  ( 3.081487911019577365E-33, -2.775557561562891967E-17, -1.000000000000000000 ) ) ;
#5798 = DIRECTION ( 'NONE',  ( -1.000000000000000000, 0.000000000000000000, 0.000000000000000000 ) ) ;
#5799 = ORIENTED_EDGE ( 'NONE', *, *, #3471, .T. ) ;
#5800 = VECTOR ( 'NONE', #6162, 1000.000000000000000 ) ;
#5801 = ADVANCED_FACE ( 'NONE', ( #144 ), #1967, .T. ) ;
#5802 = CARTESIAN_POINT ( 'NONE',  ( 5.870234470492294880E-31, -4.203179568131150526E-15, -122.9999999999999716 ) ) ;
#5803 = CARTESIAN_POINT ( 'NONE',  ( -207.8429183184026670, 119.9981648402859378, -120.0000000000000000 ) ) ;
#5804 = CIRCLE ( 'NONE', #6822, 31.52499999999999858 ) ;
#5805 = CARTESIAN_POINT ( 'NONE',  ( -10.00000000000000000, 41.99999999999999289, 10.00000000000000000 ) ) ;
#5806 = DIRECTION ( 'NONE',  ( 0.000000000000000000, 0.000000000000000000, -1.000000000000000000 ) ) ;
#5807 = VERTEX_POINT ( 'NONE', #4835 ) ;
#5808 = EDGE_CURVE ( 'NONE', #2283, #7515, #807, .T. ) ;
#5809 = LINE ( 'NONE', #364, #5499 ) ;
#5810 =( LENGTH_UNIT ( ) NAMED_UNIT ( * ) SI_UNIT ( .MILLI., .METRE. ) );
#5811 = EDGE_CURVE ( 'NONE', #6313, #1026, #2112, .T. ) ;
#5812 = EDGE_CURVE ( 'NONE', #6752, #4594, #4717, .T. ) ;
#5813 = CARTESIAN_POINT ( 'NONE',  ( -28.49999999999999645, 3.490243377569956456E-15, -3.000000000000000000 ) ) ;
#5814 = DIRECTION ( 'NONE',  ( 0.000000000000000000, 0.000000000000000000, 1.000000000000000000 ) ) ;
#5815 = CARTESIAN_POINT ( 'NONE',  ( 2.750000000000000000, -33.63777638310832430, -3.000000000000000000 ) ) ;
#5816 = ITEM_DEFINED_TRANSFORMATION ( 'NONE', 'NONE', #3472,  #7485 ) ;
#5817 = EDGE_CURVE ( 'NONE', #1298, #3552, #3336, .T. ) ;
#5818 = DIRECTION ( 'NONE',  ( 0.9845265360683707057, 0.1752355551171480841, 0.000000000000000000 ) ) ;
#5819 = ORIENTED_EDGE ( 'NONE', *, *, #48, .T. ) ;
#5820 = ORIENTED_EDGE ( 'NONE', *, *, #3423, .F. ) ;
#5821 = MANIFOLD_SOLID_BREP ( 'M10 Machine Threads Stud2', #3221 ) ;
#5822 = VERTEX_POINT ( 'NONE', #4397 ) ;
#5823 = EDGE_CURVE ( 'NONE', #578, #1051, #4212, .T. ) ;
#5824 = CARTESIAN_POINT ( 'NONE',  ( 5.690023276062392554, 5.952467836904153486, -4.569346954796190907 ) ) ;
#5825 = CARTESIAN_POINT ( 'NONE',  ( 0.000000000000000000, 0.000000000000000000, -139.9999999999999716 ) ) ;
#5826 = DIRECTION ( 'NONE',  ( 0.000000000000000000, 0.000000000000000000, 1.000000000000000000 ) ) ;
#5827 = CARTESIAN_POINT ( 'NONE',  ( -37.49999999999997868, 4.592425496802572000E-15, -82.99999999999998579 ) ) ;
#5828 = CARTESIAN_POINT ( 'NONE',  ( -63.76644452187068879, 49.96174644486002592, 0.000000000000000000 ) ) ;
#5829 = AXIS2_PLACEMENT_3D ( 'NONE', #1462, #3244, #4931 ) ;
#5830 = ORIENTED_EDGE ( 'NONE', *, *, #3207, .F. ) ;
#5831 = ORIENTED_EDGE ( 'NONE', *, *, #6493, .T. ) ;
#5832 = EDGE_LOOP ( 'NONE', ( #7210, #2108, #2854, #438, #3522, #4082 ) ) ;
#5833 = EDGE_LOOP ( 'NONE', ( #6584, #6964, #6631, #4441 ) ) ;
#5834 = CIRCLE ( 'NONE', #3696, 4.999999999999990230 ) ;
#5835 = CARTESIAN_POINT ( 'NONE',  ( -73.76644452187071010, 49.96174644486006855, -134.1720000000000255 ) ) ;
#5836 = DIRECTION ( 'NONE',  ( -1.000000000000000000, 0.000000000000000000, 0.000000000000000000 ) ) ;
#5837 = LINE ( 'NONE', #7687, #3567 ) ;
#5838 = CIRCLE ( 'NONE', #922, 6.713333333332999864 ) ;
#5839 = ORIENTED_EDGE ( 'NONE', *, *, #2068, .T. ) ;
#5840 = CARTESIAN_POINT ( 'NONE',  ( 3.200000000000007727, 0.000000000000000000, -30.30000000000000071 ) ) ;
#5841 = LINE ( 'NONE', #2231, #1390 ) ;
#5842 = AXIS2_PLACEMENT_3D ( 'NONE', #6901, #6311, #6384 ) ;
#5843 = CIRCLE ( 'NONE', #3084, 5.249999999999997335 ) ;
#5844 = CARTESIAN_POINT ( 'NONE',  ( -6.873268260756527152E-15, 0.000000000000000000, -79.99999999999995737 ) ) ;
#5845 = CARTESIAN_POINT ( 'NONE',  ( -20.63749999999999929, 0.000000000000000000, 0.000000000000000000 ) ) ;
#5846 = VERTEX_POINT ( 'NONE', #6296 ) ;
#5847 = ORIENTED_EDGE ( 'NONE', *, *, #2745, .F. ) ;
#5848 = CIRCLE ( 'NONE', #3716, 4.250000000000000000 ) ;
#5849 = STYLED_ITEM ( 'NONE', ( #5244 ), #5395 ) ;
#5850 = LINE ( 'NONE', #6444, #7270 ) ;
#5851 = DIRECTION ( 'NONE',  ( 1.000000000000000000, 0.000000000000000000, -0.000000000000000000 ) ) ;
#5852 = CARTESIAN_POINT ( 'NONE',  ( 114.7481648402869041, 207.8429183184021269, -8.673617379884035472E-15 ) ) ;
#5853 = FACE_OUTER_BOUND ( 'NONE', #7421, .T. ) ;
#5854 = CONTEXT_DEPENDENT_SHAPE_REPRESENTATION ( #4695, #5420 ) ;
#5855 = AXIS2_PLACEMENT_3D ( 'NONE', #4866, #4190, #4789 ) ;
#5856 = STYLED_ITEM ( 'NONE', ( #4449 ), #6328 ) ;
#5857 = DIRECTION ( 'NONE',  ( 1.000000000000000000, 0.000000000000000000, 0.000000000000000000 ) ) ;
#5858 = CLOSED_SHELL ( 'NONE', ( #3514, #7017, #5579, #2554, #5959, #3360, #3081, #3504, #6705, #5137, #88, #4794, #5712, #6034 ) ) ;
#5859 = ORIENTED_EDGE ( 'NONE', *, *, #3093, .F. ) ;
#5860 = ORIENTED_EDGE ( 'NONE', *, *, #6258, .T. ) ;
#5861 = ORIENTED_EDGE ( 'NONE', *, *, #2224, .T. ) ;
#5862 = AXIS2_PLACEMENT_3D ( 'NONE', #4165, #64, #4124 ) ;
#5863 = EDGE_CURVE ( 'NONE', #2201, #6741, #5599, .T. ) ;
#5864 = VECTOR ( 'NONE', #1603, 1000.000000000000000 ) ;
#5865 = CARTESIAN_POINT ( 'NONE',  ( -0.6527133886630329673, 8.860760056385741379, -4.203039949738246683 ) ) ;
#5866 = DIRECTION ( 'NONE',  ( 0.000000000000000000, 0.000000000000000000, 1.000000000000000000 ) ) ;
#5867 = CARTESIAN_POINT ( 'NONE',  ( 5.870234470492294880E-31, -4.203179568131150526E-15, -122.9999999999999716 ) ) ;
#5868 = DIRECTION ( 'NONE',  ( 1.000000000000000000, 0.000000000000000000, 0.000000000000000000 ) ) ;
#5869 = DIRECTION ( 'NONE',  ( 0.9845265360683708167, 0.1752355551171481118, -5.551115123125782086E-17 ) ) ;
#5870 = CARTESIAN_POINT ( 'NONE',  ( -74.01644452187024115, -49.96174644486060856, 0.000000000000000000 ) ) ;
#5871 = ADVANCED_FACE ( 'NONE', ( #7509 ), #252, .T. ) ;
#5872 = VERTEX_POINT ( 'NONE', #1399 ) ;
#5873 = EDGE_LOOP ( 'NONE', ( #7708, #1150, #465, #2747 ) ) ;
#5874 = AXIS2_PLACEMENT_3D ( 'NONE', #2666, #6885, #6810 ) ;
#5875 = ORIENTED_EDGE ( 'NONE', *, *, #2362, .T. ) ;
#5876 = DIRECTION ( 'NONE',  ( 0.9938725510941108787, -0.1105321318969463978, 0.000000000000000000 ) ) ;
#5877 = DIRECTION ( 'NONE',  ( 0.000000000000000000, 0.000000000000000000, 1.000000000000000000 ) ) ;
#5878 = DIRECTION ( 'NONE',  ( -0.000000000000000000, -0.000000000000000000, 1.000000000000000000 ) ) ;
#5879 = ORIENTED_EDGE ( 'NONE', *, *, #2025, .F. ) ;
#5880 = EDGE_CURVE ( 'NONE', #502, #3517, #3815, .T. ) ;
#5881 = VECTOR ( 'NONE', #1807, 1000.000000000000000 ) ;
#5882 = CARTESIAN_POINT ( 'NONE',  ( -5.857142857142855874, 7.172931252148781134E-16, 3.859999999999999876 ) ) ;
#5883 = DIRECTION ( 'NONE',  ( -1.000000000000000000, 0.000000000000000000, 0.000000000000000000 ) ) ;
#5884 = CARTESIAN_POINT ( 'NONE',  ( 3.318518101603008308, 7.321656987762871438, -4.700000000000006395 ) ) ;
#5885 = DIRECTION ( 'NONE',  ( 0.000000000000000000, 0.000000000000000000, 1.000000000000000000 ) ) ;
#5886 = VERTEX_POINT ( 'NONE', #3298 ) ;
#5887 = AXIS2_PLACEMENT_3D ( 'NONE', #7675, #7207, #1810 ) ;
#5888 = ORIENTED_EDGE ( 'NONE', *, *, #7317, .T. ) ;
#5889 = DIRECTION ( 'NONE',  ( 0.000000000000000000, 0.000000000000000000, 1.000000000000000000 ) ) ;
#5890 = CIRCLE ( 'NONE', #3005, 4.999999999999990230 ) ;
#5891 = CARTESIAN_POINT ( 'NONE',  ( 8.000000000000000000, 0.000000000000000000, 0.000000000000000000 ) ) ;
#5892 = FACE_OUTER_BOUND ( 'NONE', #5136, .T. ) ;
#5893 = CARTESIAN_POINT ( 'NONE',  ( 4.000000000000004441, 6.928203230275507885, -4.700000000000000178 ) ) ;
#5894 = ITEM_DEFINED_TRANSFORMATION ( 'NONE', 'NONE', #2969,  #7485 ) ;
#5895 = LINE ( 'NONE', #2363, #5986 ) ;
#5896 = ORIENTED_EDGE ( 'NONE', *, *, #3459, .F. ) ;
#5897 = ORIENTED_EDGE ( 'NONE', *, *, #6834, .F. ) ;
#5898 = CIRCLE ( 'NONE', #974, 37.50000000000000000 ) ;
#5899 = ORIENTED_EDGE ( 'NONE', *, *, #5477, .T. ) ;
#5900 = EDGE_CURVE ( 'NONE', #5637, #2058, #7370, .T. ) ;
#5901 = CARTESIAN_POINT ( 'NONE',  ( -8.000000000000000000, 9.797174393178825657E-16, 9.480888224575629408 ) ) ;
#5902 = AXIS2_PLACEMENT_3D ( 'NONE', #5825, #3384, #5786 ) ;
#5903 = FACE_OUTER_BOUND ( 'NONE', #543, .T. ) ;
#5904 = LINE ( 'NONE', #6456, #2497 ) ;
#5905 = CARTESIAN_POINT ( 'NONE',  ( 85.00000000000000000, 9.922618282587336580E-13, 14.69999999999999929 ) ) ;
#5906 = LINE ( 'NONE', #5827, #422 ) ;
#5907 = DIRECTION ( 'NONE',  ( 1.000000000000000000, 0.000000000000000000, 0.000000000000000000 ) ) ;
#5908 = EDGE_LOOP ( 'NONE', ( #961, #6008 ) ) ;
#5909 = CIRCLE ( 'NONE', #2765, 28.49999999999999645 ) ;
#5910 = ORIENTED_EDGE ( 'NONE', *, *, #2077, .F. ) ;
#5911 =( REPRESENTATION_RELATIONSHIP ('NONE','NONE', #1229, #5768 ) REPRESENTATION_RELATIONSHIP_WITH_TRANSFORMATION ( #5894 )SHAPE_REPRESENTATION_RELATIONSHIP( ) );
#5912 = ADVANCED_FACE ( 'NONE', ( #182 ), #4518, .F. ) ;
#5913 = VERTEX_POINT ( 'NONE', #3923 ) ;
#5914 = DIRECTION ( 'NONE',  ( 1.000000000000000000, 0.000000000000000000, 0.000000000000000000 ) ) ;
#5915 = DIRECTION ( 'NONE',  ( -1.000000000000000000, 0.000000000000000000, 0.000000000000000000 ) ) ;
#5916 = EDGE_CURVE ( 'NONE', #2423, #7135, #5737, .T. ) ;
#5917 = CIRCLE ( 'NONE', #2527, 5.249999999999991118 ) ;
#5918 = EDGE_CURVE ( 'NONE', #4626, #545, #5354, .T. ) ;
#5919 = FACE_OUTER_BOUND ( 'NONE', #4290, .T. ) ;
#5920 = EDGE_CURVE ( 'NONE', #6434, #421, #5895, .T. ) ;
#5921 = VERTEX_POINT ( 'NONE', #3490 ) ;
#5922 = VECTOR ( 'NONE', #3519, 1000.000000000000000 ) ;
#5923 = ADVANCED_FACE ( 'NONE', ( #1720 ), #1700, .T. ) ;
#5924 = DIRECTION ( 'NONE',  ( 0.000000000000000000, 0.000000000000000000, 1.000000000000000000 ) ) ;
#5925 = CARTESIAN_POINT ( 'NONE',  ( 5.000000000000000888, 6.123233995736767268E-16, -4.674599999999997202 ) ) ;
#5926 = DIRECTION ( 'NONE',  ( -1.000000000000000000, 4.286207611454020849E-16, 0.000000000000000000 ) ) ;
#5927 = CIRCLE ( 'NONE', #6559, 5.250000000000004441 ) ;
#5928 = CARTESIAN_POINT ( 'NONE',  ( -64.59444452187068464, 49.96174644486002592, 25.00000000000000000 ) ) ;
#5929 = EDGE_CURVE ( 'NONE', #6752, #6712, #2325, .T. ) ;
#5930 = VERTEX_POINT ( 'NONE', #2787 ) ;
#5931 = EDGE_LOOP ( 'NONE', ( #5483, #936, #5960, #2776 ) ) ;
#5932 = PLANE ( 'NONE',  #839 ) ;
#5933 = VECTOR ( 'NONE', #1255, 1000.000000000000000 ) ;
#5934 = CARTESIAN_POINT ( 'NONE',  ( -68.76644452187068168, 49.96174644486002592, 0.000000000000000000 ) ) ;
#5935 = DIRECTION ( 'NONE',  ( -0.000000000000000000, -0.000000000000000000, 1.000000000000000000 ) ) ;
#5936 = CARTESIAN_POINT ( 'NONE',  ( 0.000000000000000000, 150.0000000000000568, 0.000000000000000000 ) ) ;
#5937 = CARTESIAN_POINT ( 'NONE',  ( 3.200000000000008171, 0.000000000000000000, 0.000000000000000000 ) ) ;
#5938 = FACE_OUTER_BOUND ( 'NONE', #1836, .T. ) ;
#5939 = EDGE_LOOP ( 'NONE', ( #4767, #5208, #7377, #2855 ) ) ;
#5940 = VERTEX_POINT ( 'NONE', #1119 ) ;
#5941 = DIRECTION ( 'NONE',  ( 0.9845265360683708167, 0.1752355551171481118, -5.551115123125782086E-17 ) ) ;
#5942 = B_SPLINE_CURVE_WITH_KNOTS ( 'NONE', 3,
 ( #831, #124, #2581, #716, #3131, #1342 ),
 .UNSPECIFIED., .F., .F.,
 ( 4, 2, 4 ),
 ( 0.008240550023493527568, 0.01057684187039405373, 0.01291313371729457815 ),
 .UNSPECIFIED. ) ;
#5943 = DIRECTION ( 'NONE',  ( 1.000000000000000000, 0.000000000000000000, 0.000000000000000000 ) ) ;
#5944 = DIRECTION ( 'NONE',  ( 0.9412010056177179118, 0.3378471059875997051, 0.000000000000000000 ) ) ;
#5945 = DIRECTION ( 'NONE',  ( -3.101873702526156189E-17, 3.926253788359931981E-17, -0.9999999999999998890 ) ) ;
#5946 = CARTESIAN_POINT ( 'NONE',  ( -3.199999999999994404, 0.000000000000000000, -37.50000000000000000 ) ) ;
#5947 = DIRECTION ( 'NONE',  ( -5.551115123125782702E-17, 0.000000000000000000, -1.000000000000000000 ) ) ;
#5948 = ORIENTED_EDGE ( 'NONE', *, *, #3750, .F. ) ;
#5949 = VECTOR ( 'NONE', #6686, 1000.000000000000000 ) ;
#5950 = VERTEX_POINT ( 'NONE', #6415 ) ;
#5951 = AXIS2_PLACEMENT_3D ( 'NONE', #4870, #6725, #5500 ) ;
#5952 = ORIENTED_EDGE ( 'NONE', *, *, #6226, .F. ) ;
#5953 = CARTESIAN_POINT ( 'NONE',  ( 0.000000000000000000, 0.000000000000000000, 10.00000000000000000 ) ) ;
#5954 = CARTESIAN_POINT ( 'NONE',  ( -20.63749999999999574, 4.405666859932604686E-15, 35.97500000000000853 ) ) ;
#5955 =( NAMED_UNIT ( * ) SI_UNIT ( $, .STERADIAN. ) SOLID_ANGLE_UNIT ( ) );
#5956 = AXIS2_PLACEMENT_3D ( 'NONE', #6199, #7491, #163 ) ;
#5957 = PRODUCT_DEFINITION_FORMATION_WITH_SPECIFIED_SOURCE ( 'ANY', '', #1837, .NOT_KNOWN. ) ;
#5958 = FACE_OUTER_BOUND ( 'NONE', #2270, .T. ) ;
#5959 = ADVANCED_FACE ( 'NONE', ( #370 ), #4115, .T. ) ;
#5960 = ORIENTED_EDGE ( 'NONE', *, *, #2648, .T. ) ;
#5961 = ORIENTED_EDGE ( 'NONE', *, *, #3357, .F. ) ;
#5962 = AXIS2_PLACEMENT_3D ( 'NONE', #1762, #2207, #4152 ) ;
#5963 = ADVANCED_FACE ( 'NONE', ( #5181 ), #5226, .T. ) ;
#5964 = EDGE_CURVE ( 'NONE', #2183, #5972, #4592, .T. ) ;
#5965 = DIRECTION ( 'NONE',  ( 0.000000000000000000, -0.000000000000000000, -1.000000000000000000 ) ) ;
#5966 = DIRECTION ( 'NONE',  ( -0.000000000000000000, -0.000000000000000000, 1.000000000000000000 ) ) ;
#5967 = DIRECTION ( 'NONE',  ( -0.000000000000000000, -0.000000000000000000, -1.000000000000000000 ) ) ;
#5968 = DIRECTION ( 'NONE',  ( 0.000000000000000000, 0.000000000000000000, 1.000000000000000000 ) ) ;
#5969 = EDGE_LOOP ( 'NONE', ( #2977, #4583, #5157, #925 ) ) ;
#5970 = EDGE_LOOP ( 'NONE', ( #72, #4480, #334, #2841 ) ) ;
#5971 = EDGE_CURVE ( 'NONE', #6819, #7320, #5722, .T. ) ;
#5972 = VERTEX_POINT ( 'NONE', #1039 ) ;
#5973 = VECTOR ( 'NONE', #3161, 1000.000000000000000 ) ;
#5974 = VECTOR ( 'NONE', #5772, 1000.000000000000000 ) ;
#5975 = DIRECTION ( 'NONE',  ( 1.000000000000000000, -4.286207611454020849E-16, 0.000000000000000000 ) ) ;
#5976 = DIRECTION ( 'NONE',  ( 1.000000000000000000, 0.000000000000000000, 0.000000000000000000 ) ) ;
#5977 = DIRECTION ( 'NONE',  ( 1.000000000000000000, 0.000000000000000000, 0.000000000000000000 ) ) ;
#5978 = DIRECTION ( 'NONE',  ( 0.000000000000000000, 0.000000000000000000, 1.000000000000000000 ) ) ;
#5979 = CARTESIAN_POINT ( 'NONE',  ( 129.9038105676649764, 75.00000000000153477, 10.00000000000000000 ) ) ;
#5980 = CONTEXT_DEPENDENT_SHAPE_REPRESENTATION ( #1472, #2475 ) ;
#5981 = CARTESIAN_POINT ( 'NONE',  ( -105.4635834177236546, -106.6650485055571380, 10.00000000000000000 ) ) ;
#5982 = ORIENTED_EDGE ( 'NONE', *, *, #470, .T. ) ;
#5983 =( GEOMETRIC_REPRESENTATION_CONTEXT ( 3 ) GLOBAL_UNCERTAINTY_ASSIGNED_CONTEXT ( ( #5512 ) ) GLOBAL_UNIT_ASSIGNED_CONTEXT ( ( #4614, #2883, #2300 ) ) REPRESENTATION_CONTEXT ( 'NONE', 'WORKASPACE' ) );
#5984 = ORIENTED_EDGE ( 'NONE', *, *, #2061, .F. ) ;
#5985 = CARTESIAN_POINT ( 'NONE',  ( -3.319543390096037161, 7.321065037175422674, -4.683111142572233376 ) ) ;
#5986 = VECTOR ( 'NONE', #6963, 1000.000000000000000 ) ;
#5987 = LINE ( 'NONE', #4759, #1615 ) ;
#5988 = DIRECTION ( 'NONE',  ( 1.000000000000000000, 0.000000000000000000, 0.000000000000000000 ) ) ;
#5989 = CARTESIAN_POINT ( 'NONE',  ( 4.793225973945551641E-15, 0.000000000000000000, -86.49999999999998579 ) ) ;
#5990 = PRODUCT_DEFINITION_SHAPE ( 'NONE', 'NONE',  #7790 ) ;
#5991 = CARTESIAN_POINT ( 'NONE',  ( -4.586480920263581673, -37.21846574978686562, 0.000000000000000000 ) ) ;
#5992 = ORIENTED_EDGE ( 'NONE', *, *, #3212, .T. ) ;
#5993 = AXIS2_PLACEMENT_3D ( 'NONE', #414, #2251, #2835 ) ;
#5994 = EDGE_LOOP ( 'NONE', ( #3229, #6613, #5376, #6388 ) ) ;
#5995 = ORIENTED_EDGE ( 'NONE', *, *, #7071, .F. ) ;
#5996 = DIRECTION ( 'NONE',  ( 0.000000000000000000, 0.000000000000000000, 1.000000000000000000 ) ) ;
#5997 = CARTESIAN_POINT ( 'NONE',  ( -1.734723475976807094E-15, 9.237604307034017026, -0.7145311798163319628 ) ) ;
#5998 = FILL_AREA_STYLE ('',( #1294 ) ) ;
#5999 = CARTESIAN_POINT ( 'NONE',  ( -73.76644452187066747, 49.96174644486002592, 0.000000000000000000 ) ) ;
#6000 = ORIENTED_EDGE ( 'NONE', *, *, #7359, .T. ) ;
#6001 = COLOUR_RGB ( '',1.000000000000000000, 0.9490196078431372140, 0.9098039215686274384 ) ;
#6002 = VERTEX_POINT ( 'NONE', #2243 ) ;
#6003 = PRODUCT_DEFINITION ( 'UNKNOWN', '', #6841, #4710 ) ;
#6004 = DIRECTION ( 'NONE',  ( 1.000000000000000000, 0.000000000000000000, 0.000000000000000000 ) ) ;
#6005 = CIRCLE ( 'NONE', #3982, 1.250000000000000222 ) ;
#6006 = PLANE ( 'NONE',  #1612 ) ;
#6007 = CARTESIAN_POINT ( 'NONE',  ( -37.49999999999997868, 4.592425496802572000E-15, -82.99999999999998579 ) ) ;
#6008 = ORIENTED_EDGE ( 'NONE', *, *, #7544, .T. ) ;
#6009 = EDGE_CURVE ( 'NONE', #6903, #6492, #5848, .T. ) ;
#6010 = EDGE_LOOP ( 'NONE', ( #3686, #6723, #6287, #1899, #5784, #4303 ) ) ;
#6011 = AXIS2_PLACEMENT_3D ( 'NONE', #2737, #5059, #174 ) ;
#6012 = ORIENTED_EDGE ( 'NONE', *, *, #1981, .F. ) ;
#6013 = CARTESIAN_POINT ( 'NONE',  ( 9.568665290872615969, -28.43309066125680928, -119.9999999999999716 ) ) ;
#6014 = DIRECTION ( 'NONE',  ( 0.000000000000000000, 0.000000000000000000, 1.000000000000000000 ) ) ;
#6015 = CARTESIAN_POINT ( 'NONE',  ( -73.76644452187066747, 49.96174644486002592, -64.17200000000001125 ) ) ;
#6016 = CARTESIAN_POINT ( 'NONE',  ( 0.000000000000000000, 150.0000000000000568, 10.00000000000000000 ) ) ;
#6017 = EDGE_CURVE ( 'NONE', #1335, #7413, #4593, .T. ) ;
#6018 = CIRCLE ( 'NONE', #2618, 6.713333333332999864 ) ;
#6019 = DIRECTION ( 'NONE',  ( 0.000000000000000000, 0.000000000000000000, 1.000000000000000000 ) ) ;
#6020 = ORIENTED_EDGE ( 'NONE', *, *, #616, .T. ) ;
#6021 =( REPRESENTATION_RELATIONSHIP ('NONE','NONE', #1229, #7725 ) REPRESENTATION_RELATIONSHIP_WITH_TRANSFORMATION ( #1878 )SHAPE_REPRESENTATION_RELATIONSHIP( ) );
#6022 = ADVANCED_FACE ( 'NONE', ( #5938 ), #7707, .T. ) ;
#6023 = VECTOR ( 'NONE', #5223, 1000.000000000000000 ) ;
#6024 = DIRECTION ( 'NONE',  ( -1.000000000000000000, 1.586032892321652482E-16, 0.000000000000000000 ) ) ;
#6025 = EDGE_CURVE ( 'NONE', #2491, #3391, #1598, .T. ) ;
#6026 = DIRECTION ( 'NONE',  ( -0.8191520442889924647, 0.000000000000000000, -0.5735764363510451602 ) ) ;
#6027 = CARTESIAN_POINT ( 'NONE',  ( 0.000000000000000000, 0.000000000000000000, -90.00000000000000000 ) ) ;
#6028 = DIRECTION ( 'NONE',  ( 0.9831827147437113279, 0.1826246134265212540, 1.931932416011734352E-18 ) ) ;
#6029 = DIRECTION ( 'NONE',  ( -1.586032892321652729E-16, -1.000000000000000000, 0.000000000000000000 ) ) ;
#6030 = CARTESIAN_POINT ( 'NONE',  ( 105.4635834177229157, 106.6650485055578912, 5.000000000000000000 ) ) ;
#6031 = UNCERTAINTY_MEASURE_WITH_UNIT (LENGTH_MEASURE( 1.000000000000000082E-05 ), #7527, 'distance_accuracy_value', 'NONE');
#6032 = CARTESIAN_POINT ( 'NONE',  ( -73.76644452187066747, 49.96174644486002592, 24.17200000000001125 ) ) ;
#6033 = VECTOR ( 'NONE', #7066, 1000.000000000000000 ) ;
#6034 = ADVANCED_FACE ( 'NONE', ( #7122 ), #6529, .T. ) ;
#6035 = EDGE_LOOP ( 'NONE', ( #5184, #661, #7671, #650 ) ) ;
#6036 = ORIENTED_EDGE ( 'NONE', *, *, #3747, .T. ) ;
#6037 = ORIENTED_EDGE ( 'NONE', *, *, #601, .T. ) ;
#6038 = CARTESIAN_POINT ( 'NONE',  ( 3.500000000000006661, 0.000000000000000000, 0.000000000000000000 ) ) ;
#6039 =( LENGTH_UNIT ( ) NAMED_UNIT ( * ) SI_UNIT ( .MILLI., .METRE. ) );
#6040 = CARTESIAN_POINT ( 'NONE',  ( -68.76644452187068168, 49.96174644486002592, -65.00000000000000000 ) ) ;
#6041 = AXIS2_PLACEMENT_3D ( 'NONE', #1198, #2434, #7275 ) ;
#6042 = EDGE_LOOP ( 'NONE', ( #3341, #2221, #4998 ) ) ;
#6043 = ORIENTED_EDGE ( 'NONE', *, *, #400, .T. ) ;
#6044 = VECTOR ( 'NONE', #4215, 1000.000000000000000 ) ;
#6045 = DIRECTION ( 'NONE',  ( -0.000000000000000000, -0.000000000000000000, 1.000000000000000000 ) ) ;
#6046 = LINE ( 'NONE', #1302, #5645 ) ;
#6047 = PLANE ( 'NONE',  #5068 ) ;
#6048 = ORIENTED_EDGE ( 'NONE', *, *, #4462, .F. ) ;
#6049 = VECTOR ( 'NONE', #2054, 1000.000000000000000 ) ;
#6050 = ORIENTED_EDGE ( 'NONE', *, *, #2590, .F. ) ;
#6051 = PRODUCT_DEFINITION_SHAPE ( 'NONE', 'NONE',  #7787 ) ;
#6052 = DIRECTION ( 'NONE',  ( 1.000000000000000000, 0.000000000000000000, -0.000000000000000000 ) ) ;
#6053 = DIRECTION ( 'NONE',  ( -0.000000000000000000, -0.000000000000000000, 1.000000000000000000 ) ) ;
#6054 = CIRCLE ( 'NONE', #1134, 28.50000000000000711 ) ;
#6055 = CARTESIAN_POINT ( 'NONE',  ( 21.01644452187122170, -80.83980388508783221, 10.00000000000000000 ) ) ;
#6056 = CARTESIAN_POINT ( 'NONE',  ( -8.000000000000000000, 4.618802153517003184, -4.700000000000000178 ) ) ;
#6057 = ITEM_DEFINED_TRANSFORMATION ( 'NONE', 'NONE', #3220,  #7485 ) ;
#6058 = CARTESIAN_POINT ( 'NONE',  ( -63.76644452187068879, 49.96174644486002592, -40.00000000000000000 ) ) ;
#6059 = EDGE_LOOP ( 'NONE', ( #304, #6316, #5593, #4926 ) ) ;
#6060 = ADVANCED_FACE ( 'NONE', ( #2863 ), #3464, .F. ) ;
#6061 = CIRCLE ( 'NONE', #382, 28.50000000000000711 ) ;
#6062 = EDGE_CURVE ( 'NONE', #2536, #3320, #1064, .T. ) ;
#6063 = ADVANCED_FACE ( 'NONE', ( #1079 ), #6866, .T. ) ;
#6064 = DIRECTION ( 'NONE',  ( -1.000000000000000000, -0.000000000000000000, -0.000000000000000000 ) ) ;
#6065 = EDGE_CURVE ( 'NONE', #3701, #1483, #3844, .T. ) ;
#6066 = LINE ( 'NONE', #7245, #5146 ) ;
#6067 = CARTESIAN_POINT ( 'NONE',  ( -68.76644452187024115, -49.96174644486060856, 10.00000000000000000 ) ) ;
#6068 = DIRECTION ( 'NONE',  ( -0.4067366430757911044, -0.9135454576426049744, 0.000000000000000000 ) ) ;
#6069 = AXIS2_PLACEMENT_3D ( 'NONE', #2053, #5746, #7517 ) ;
#6070 = CARTESIAN_POINT ( 'NONE',  ( 279.9963296805736945, -6.783120157456498832E-12, 10.00000000000000000 ) ) ;
#6071 = DIRECTION ( 'NONE',  ( -0.000000000000000000, -0.000000000000000000, 1.000000000000000000 ) ) ;
#6072 = VERTEX_POINT ( 'NONE', #4273 ) ;
#6073 = VERTEX_POINT ( 'NONE', #6612 ) ;
#6074 = EDGE_CURVE ( 'NONE', #3671, #6644, #3572, .T. ) ;
#6075 = EDGE_LOOP ( 'NONE', ( #4619, #1182, #3865, #2472 ) ) ;
#6076 = DIRECTION ( 'NONE',  ( -0.000000000000000000, -0.000000000000000000, 1.000000000000000000 ) ) ;
#6077 =( NAMED_UNIT ( * ) SI_UNIT ( $, .STERADIAN. ) SOLID_ANGLE_UNIT ( ) );
#6078 = DIRECTION ( 'NONE',  ( 0.9412010056177179118, 0.3378471059875997051, 0.000000000000000000 ) ) ;
#6079 = ORIENTED_EDGE ( 'NONE', *, *, #2924, .T. ) ;
#6080 = ORIENTED_EDGE ( 'NONE', *, *, #128, .F. ) ;
#6081 = AXIS2_PLACEMENT_3D ( 'NONE', #5171, #6476, #7574 ) ;
#6082 = CARTESIAN_POINT ( 'NONE',  ( 8.000000000000000000, 0.000000000000000000, 2.573333333333333695 ) ) ;
#6083 = FACE_OUTER_BOUND ( 'NONE', #6593, .T. ) ;
#6084 = CARTESIAN_POINT ( 'NONE',  ( 9.090232026328989079, -27.01143612819398143, -119.9999999999999716 ) ) ;
#6085 = CIRCLE ( 'NONE', #5451, 8.000000000000000000 ) ;
#6086 = VERTEX_POINT ( 'NONE', #5981 ) ;
#6087 = PRODUCT_DEFINITION_FORMATION_WITH_SPECIFIED_SOURCE ( 'ANY', '', #6750, .NOT_KNOWN. ) ;
#6088 = ORIENTED_EDGE ( 'NONE', *, *, #3398, .T. ) ;
#6089 = DIRECTION ( 'NONE',  ( 0.000000000000000000, 1.000000000000000000, -1.224646799147353207E-16 ) ) ;
#6090 = FACE_OUTER_BOUND ( 'NONE', #3975, .T. ) ;
#6091 = AXIS2_PLACEMENT_3D ( 'NONE', #6205, #3680, #2510 ) ;
#6092 = FACE_BOUND ( 'NONE', #206, .T. ) ;
#6093 = DIRECTION ( 'NONE',  ( 0.000000000000000000, -1.000000000000000000, 0.000000000000000000 ) ) ;
#6094 = CONTEXT_DEPENDENT_SHAPE_REPRESENTATION ( #7620, #633 ) ;
#6095 = DIRECTION ( 'NONE',  ( 0.000000000000000000, 0.000000000000000000, -1.000000000000000000 ) ) ;
#6096 = EDGE_LOOP ( 'NONE', ( #7109, #5518, #6548, #7126 ) ) ;
#6097 = CARTESIAN_POINT ( 'NONE',  ( 3.499999999999996003, 4.316879966994419494E-15, 35.25000000000000000 ) ) ;
#6098 = DIRECTION ( 'NONE',  ( -0.000000000000000000, -0.000000000000000000, 1.000000000000000000 ) ) ;
#6099 = CARTESIAN_POINT ( 'NONE',  ( 8.000000000000000000, 0.000000000000000000, 0.000000000000000000 ) ) ;
#6100 = DIRECTION ( 'NONE',  ( 0.9412010056177182449, 0.3378471059875998161, 1.703375277368108108E-17 ) ) ;
#6101 = AXIS2_PLACEMENT_3D ( 'NONE', #7755, #2291, #2956 ) ;
#6102 = CIRCLE ( 'NONE', #1824, 4.999999999999990230 ) ;
#6103 = LINE ( 'NONE', #695, #3208 ) ;
#6104 = FACE_OUTER_BOUND ( 'NONE', #2177, .T. ) ;
#6105 = DIRECTION ( 'NONE',  ( 0.01999999999999999001, -0.9997999799959990108, 0.000000000000000000 ) ) ;
#6106 = ORIENTED_EDGE ( 'NONE', *, *, #6589, .T. ) ;
#6107 = ADVANCED_FACE ( 'NONE', ( #3061, #6570 ), #3614, .F. ) ;
#6108 = ORIENTED_EDGE ( 'NONE', *, *, #2175, .F. ) ;
#6109 = AXIS2_PLACEMENT_3D ( 'NONE', #4077, #960, #5818 ) ;
#6110 = ORIENTED_EDGE ( 'NONE', *, *, #6753, .F. ) ;
#6111 = LINE ( 'NONE', #3044, #5933 ) ;
#6112 =( NAMED_UNIT ( * ) SI_UNIT ( $, .STERADIAN. ) SOLID_ANGLE_UNIT ( ) );
#6113 = FILL_AREA_STYLE ('',( #6666 ) ) ;
#6114 = DIRECTION ( 'NONE',  ( 1.000000000000000000, 0.000000000000000000, 0.000000000000000000 ) ) ;
#6115 = ADVANCED_FACE ( 'NONE', ( #4237 ), #433, .F. ) ;
#6116 =( GEOMETRIC_REPRESENTATION_CONTEXT ( 3 ) GLOBAL_UNCERTAINTY_ASSIGNED_CONTEXT ( ( #6754 ) ) GLOBAL_UNIT_ASSIGNED_CONTEXT ( ( #7406, #5668, #741 ) ) REPRESENTATION_CONTEXT ( 'NONE', 'WORKASPACE' ) );
#6117 = PRODUCT_DEFINITION_SHAPE ( 'NONE', 'NONE',  #7794 ) ;
#6118 = ORIENTED_EDGE ( 'NONE', *, *, #1688, .T. ) ;
#6119 = ORIENTED_EDGE ( 'NONE', *, *, #2657, .T. ) ;
#6120 = CLOSED_SHELL ( 'NONE', ( #658, #6882, #6787, #5145, #6448, #399, #1620, #3326, #6060, #3040, #4483, #2882, #3141, #4997, #1242, #5801, #4617, #1333, #764, #6115, #3455, #890, #798, #2426, #1880, #4900, #704, #4555, #7590, #5912, #1104 ) ) ;
#6121 = DIRECTION ( 'NONE',  ( 0.000000000000000000, 0.000000000000000000, -1.000000000000000000 ) ) ;
#6122 = DIRECTION ( 'NONE',  ( 0.000000000000000000, -1.000000000000000000, 0.000000000000000000 ) ) ;
#6123 = CARTESIAN_POINT ( 'NONE',  ( 119.9981648402866341, 207.8429183184022122, -120.0000000000000000 ) ) ;
#6124 = CIRCLE ( 'NONE', #6632, 1.286666666666999914 ) ;
#6125 = CARTESIAN_POINT ( 'NONE',  ( 213.0929183184020701, 119.9981648402868331, 10.00000000000000178 ) ) ;
#6126 = EDGE_LOOP ( 'NONE', ( #3230, #1203, #1131, #2246 ) ) ;
#6127 = EDGE_CURVE ( 'NONE', #4490, #746, #1444, .T. ) ;
#6128 = ORIENTED_EDGE ( 'NONE', *, *, #7115, .T. ) ;
#6129 = VECTOR ( 'NONE', #1231, 1000.000000000000000 ) ;
#6130 = FACE_OUTER_BOUND ( 'NONE', #999, .T. ) ;
#6131 = DIRECTION ( 'NONE',  ( -0.000000000000000000, -0.000000000000000000, 1.000000000000000000 ) ) ;
#6132 = CARTESIAN_POINT ( 'NONE',  ( 0.000000000000000000, 0.000000000000000000, -122.9999999999999716 ) ) ;
#6133 = CARTESIAN_POINT ( 'NONE',  ( 145.1064334105730893, 38.00161816111175739, 0.000000000000000000 ) ) ;
#6134 = CONTEXT_DEPENDENT_SHAPE_REPRESENTATION ( #1067, #2031 ) ;
#6135 = DIRECTION ( 'NONE',  ( 0.000000000000000000, 0.000000000000000000, -1.000000000000000000 ) ) ;
#6136 = ORIENTED_EDGE ( 'NONE', *, *, #5678, .T. ) ;
#6137 = VECTOR ( 'NONE', #3292, 1000.000000000000000 ) ;
#6138 = CARTESIAN_POINT ( 'NONE',  ( 85.00000000000000000, 9.720002580593245511E-13, 10.00000000000000000 ) ) ;
#6139 = AXIS2_PLACEMENT_3D ( 'NONE', #6334, #6961, #1554 ) ;
#6140 = DIRECTION ( 'NONE',  ( -0.000000000000000000, -0.000000000000000000, 1.000000000000000000 ) ) ;
#6141 = FACE_OUTER_BOUND ( 'NONE', #1618, .T. ) ;
#6142 = PRODUCT_CONTEXT ( 'NONE', #567, 'mechanical' ) ;
#6143 = LINE ( 'NONE', #2447, #2587 ) ;
#6144 = CARTESIAN_POINT ( 'NONE',  ( 30.00000000000000000, 0.000000000000000000, 10.00000000000000000 ) ) ;
#6145 = FACE_BOUND ( 'NONE', #4965, .T. ) ;
#6146 = ORIENTED_EDGE ( 'NONE', *, *, #3403, .T. ) ;
#6147 = AXIS2_PLACEMENT_3D ( 'NONE', #5534, #5571, #20 ) ;
#6148 = VERTEX_POINT ( 'NONE', #1202 ) ;
#6149 = PRODUCT_RELATED_PRODUCT_CATEGORY ( 'part', '', ( #2099 ) ) ;
#6150 = ORIENTED_EDGE ( 'NONE', *, *, #6959, .T. ) ;
#6151 = FACE_OUTER_BOUND ( 'NONE', #6428, .T. ) ;
#6152 =( NAMED_UNIT ( * ) SI_UNIT ( $, .STERADIAN. ) SOLID_ANGLE_UNIT ( ) );
#6153 = AXIS2_PLACEMENT_3D ( 'NONE', #4737, #4145, #6558 ) ;
#6154 = CARTESIAN_POINT ( 'NONE',  ( 0.000000000000000000, 0.000000000000000000, 3.859999999999999876 ) ) ;
#6155 = ORIENTED_EDGE ( 'NONE', *, *, #1691, .T. ) ;
#6156 = EDGE_LOOP ( 'NONE', ( #5551, #6791, #2384, #4967 ) ) ;
#6157 = ADVANCED_FACE ( 'NONE', ( #7319 ), #6650, .T. ) ;
#6158 = EDGE_LOOP ( 'NONE', ( #5948, #5471 ) ) ;
#6159 = VECTOR ( 'NONE', #2214, 1000.000000000000000 ) ;
#6160 = EDGE_CURVE ( 'NONE', #6072, #3312, #6617, .T. ) ;
#6161 = EDGE_CURVE ( 'NONE', #293, #7135, #60, .T. ) ;
#6162 = DIRECTION ( 'NONE',  ( -0.000000000000000000, -0.000000000000000000, 1.000000000000000000 ) ) ;
#6163 = VECTOR ( 'NONE', #929, 1000.000000000000114 ) ;
#6164 = EDGE_CURVE ( 'NONE', #688, #147, #3214, .T. ) ;
#6165 = CARTESIAN_POINT ( 'NONE',  ( 199.9963296805737230, -4.860399174643270382E-12, 10.00000000000000000 ) ) ;
#6166 = CARTESIAN_POINT ( 'NONE',  ( 90.25000000000001421, 9.720002580593245511E-13, 10.00000000000000000 ) ) ;
#6167 = VERTEX_POINT ( 'NONE', #5497 ) ;
#6168 = AXIS2_PLACEMENT_3D ( 'NONE', #6485, #7705, #4706 ) ;
#6169 = EDGE_CURVE ( 'NONE', #3008, #3001, #1314, .T. ) ;
#6170 = EDGE_LOOP ( 'NONE', ( #3821, #6234, #3092, #5592 ) ) ;
#6171 = FACE_OUTER_BOUND ( 'NONE', #1650, .T. ) ;
#6172 = CARTESIAN_POINT ( 'NONE',  ( 350.0000000000000000, -300.0000000000000000, -82.99999999999998579 ) ) ;
#6173 = FACE_BOUND ( 'NONE', #7376, .T. ) ;
#6174 = CIRCLE ( 'NONE', #5413, 5.857142857142856762 ) ;
#6175 = LINE ( 'NONE', #4389, #4558 ) ;
#6176 = ORIENTED_EDGE ( 'NONE', *, *, #1914, .F. ) ;
#6177 = CARTESIAN_POINT ( 'NONE',  ( 29.99999999999999289, 2.565854121688507820E-48, -119.9999999999999716 ) ) ;
#6178=STYLED_ITEM('',(#7837),#3145);
#6179 = DIRECTION ( 'NONE',  ( 0.7071067811865504593, 8.659560562354968603E-17, -0.7071067811865445751 ) ) ;
#6180 = FACE_OUTER_BOUND ( 'NONE', #5931, .T. ) ;
#6181 = DIRECTION ( 'NONE',  ( 1.000000000000000000, 0.000000000000000000, 0.000000000000000000 ) ) ;
#6182 = PRODUCT_CONTEXT ( 'NONE', #2446, 'mechanical' ) ;
#6183 = PRODUCT_DEFINITION_SHAPE ( 'NONE', 'NONE',  #7800 ) ;
#6184 = CARTESIAN_POINT ( 'NONE',  ( -20.63749999999999574, 0.000000000000000000, -35.25000000000000000 ) ) ;
#6185 = FACE_OUTER_BOUND ( 'NONE', #2847, .T. ) ;
#6186 = CIRCLE ( 'NONE', #1904, 4.171999999999995268 ) ;
#6187 = ORIENTED_EDGE ( 'NONE', *, *, #6442, .T. ) ;
#6188 = ORIENTED_EDGE ( 'NONE', *, *, #1958, .F. ) ;
#6189 = VERTEX_POINT ( 'NONE', #7279 ) ;
#6190 = AXIS2_PLACEMENT_3D ( 'NONE', #6585, #7373, #1175 ) ;
#6191 = PLANE ( 'NONE',  #7696 ) ;
#6192 =( NAMED_UNIT ( * ) PLANE_ANGLE_UNIT ( ) SI_UNIT ( $, .RADIAN. ) );
#6193 = DIRECTION ( 'NONE',  ( -0.000000000000000000, 1.000000000000000000, 0.000000000000000000 ) ) ;
#6194 = ORIENTED_EDGE ( 'NONE', *, *, #1183, .F. ) ;
#6195 = ORIENTED_EDGE ( 'NONE', *, *, #6834, .T. ) ;
#6196 = DIRECTION ( 'NONE',  ( 1.000000000000000000, 0.000000000000000000, 0.000000000000000000 ) ) ;
#6197 = EDGE_CURVE ( 'NONE', #4638, #5113, #137, .T. ) ;
#6198 = DIRECTION ( 'NONE',  ( 0.000000000000000000, -0.000000000000000000, 1.000000000000000000 ) ) ;
#6199 = CARTESIAN_POINT ( 'NONE',  ( 0.000000000000000000, 1.484218055610305731, 0.000000000000000000 ) ) ;
#6200 = VERTEX_POINT ( 'NONE', #725 ) ;
#6201 = EDGE_CURVE ( 'NONE', #7291, #913, #7201, .T. ) ;
#6202 = CIRCLE ( 'NONE', #2804, 5.250000000000004441 ) ;
#6203 = EDGE_CURVE ( 'NONE', #3664, #2220, #535, .T. ) ;
#6204 = CARTESIAN_POINT ( 'NONE',  ( -2.644994884459111795, 7.710515798486362371, -0.08224679563971296070 ) ) ;
#6205 = CARTESIAN_POINT ( 'NONE',  ( 0.000000000000000000, 0.000000000000000000, -119.9999999999999858 ) ) ;
#6206 = LINE ( 'NONE', #4388, #2506 ) ;
#6207 = VECTOR ( 'NONE', #6209, 1000.000000000000000 ) ;
#6208 = UNCERTAINTY_MEASURE_WITH_UNIT (LENGTH_MEASURE( 1.000000000000000082E-05 ), #6695, 'distance_accuracy_value', 'NONE');
#6209 = DIRECTION ( 'NONE',  ( -0.3189555096957539804, 0.9477696887085605981, -2.581026109104742702E-17 ) ) ;
#6210 = CARTESIAN_POINT ( 'NONE',  ( -2.750000000000000000, -33.63777638310832430, -3.000000000000000000 ) ) ;
#6211 = EDGE_CURVE ( 'NONE', #5335, #4251, #5425, .T. ) ;
#6212 = ORIENTED_EDGE ( 'NONE', *, *, #7331, .T. ) ;
#6213 = APPLICATION_CONTEXT ( 'automotive_design' ) ;
#6214 = CARTESIAN_POINT ( 'NONE',  ( -29.99999999999999289, 3.673940397442058389E-15, -119.9999999999999716 ) ) ;
#6215 = VECTOR ( 'NONE', #1890, 1000.000000000000000 ) ;
#6216 = DIRECTION ( 'NONE',  ( 1.000000000000000000, 0.000000000000000000, 0.000000000000000000 ) ) ;
#6217 = DIRECTION ( 'NONE',  ( 0.000000000000000000, 1.224646799147359124E-16, 1.000000000000000000 ) ) ;
#6218 = LINE ( 'NONE', #3854, #3000 ) ;
#6219 = PRODUCT_CONTEXT ( 'NONE', #1624, 'mechanical' ) ;
#6220 = DIRECTION ( 'NONE',  ( -0.000000000000000000, -0.000000000000000000, 1.000000000000000000 ) ) ;
#6221 = CARTESIAN_POINT ( 'NONE',  ( -68.76644452187068168, 49.96174644486002592, -40.00000000000000000 ) ) ;
#6222 = AXIS2_PLACEMENT_3D ( 'NONE', #4216, #1897, #6078 ) ;
#6223 = VERTEX_POINT ( 'NONE', #21 ) ;
#6224 = ORIENTED_EDGE ( 'NONE', *, *, #6753, .T. ) ;
#6225 = ORIENTED_EDGE ( 'NONE', *, *, #159, .F. ) ;
#6226 = EDGE_CURVE ( 'NONE', #2100, #6929, #2438, .T. ) ;
#6227 = ORIENTED_EDGE ( 'NONE', *, *, #2279, .T. ) ;
#6228 = CONICAL_SURFACE ( 'NONE', #7602, 4.999999999999990230, 0.7853981633974524978 ) ;
#6229 = CARTESIAN_POINT ( 'NONE',  ( -2.750000000000000000, -33.63777638310832430, -3.000000000000000000 ) ) ;
#6230 = CARTESIAN_POINT ( 'NONE',  ( 5.777789833161707559E-31, -4.119912841284263785E-15, -119.9999999999999716 ) ) ;
#6231 = SHAPE_REPRESENTATION_RELATIONSHIP ( 'NONE' , 'NONE' ,  #2306, #6328 ) ;
#6232 = FACE_OUTER_BOUND ( 'NONE', #6592, .T. ) ;
#6233 = COLOUR_RGB ( '',1.000000000000000000, 0.9490196078431372140, 0.9098039215686274384 ) ;
#6234 = ORIENTED_EDGE ( 'NONE', *, *, #795, .F. ) ;
#6235 = ORIENTED_EDGE ( 'NONE', *, *, #327, .T. ) ;
#6236 = LINE ( 'NONE', #196, #1783 ) ;
#6238 = AXIS2_PLACEMENT_3D ( 'NONE', #3964, #3142, #1915 ) ;
#6237 = SURFACE_SIDE_STYLE ('',( #3830 ) ) ;
#6239 =( GEOMETRIC_REPRESENTATION_CONTEXT ( 3 ) GLOBAL_UNCERTAINTY_ASSIGNED_CONTEXT ( ( #6514 ) ) GLOBAL_UNIT_ASSIGNED_CONTEXT ( ( #1933, #1819, #6077 ) ) REPRESENTATION_CONTEXT ( 'NONE', 'WORKASPACE' ) );
#6240 = CARTESIAN_POINT ( 'NONE',  ( -105.4635834177236546, -106.6650485055571380, 5.000000000000000000 ) ) ;
#6241 = DIRECTION ( 'NONE',  ( 0.000000000000000000, 0.000000000000000000, -1.000000000000000000 ) ) ;
#6242 = ORIENTED_EDGE ( 'NONE', *, *, #5000, .T. ) ;
#6243 = AXIS2_PLACEMENT_3D ( 'NONE', #4874, #693, #6028 ) ;
#6244 = PRODUCT_DEFINITION_SHAPE ( 'NONE', 'NONE',  #7394 ) ;
#6245 = DIRECTION ( 'NONE',  ( -1.000000000000000000, -8.881784197001252323E-16, 0.000000000000000000 ) ) ;
#6246 = FACE_BOUND ( 'NONE', #1938, .T. ) ;
#6247 = DIRECTION ( 'NONE',  ( 1.000000000000000000, 0.000000000000000000, 0.000000000000000000 ) ) ;
#6248 = DIRECTION ( 'NONE',  ( -0.000000000000000000, -0.000000000000000000, 1.000000000000000000 ) ) ;
#6249 = ORIENTED_EDGE ( 'NONE', *, *, #2628, .F. ) ;
#6250 = CIRCLE ( 'NONE', #1461, 37.50000000000000000 ) ;
#6251 = LINE ( 'NONE', #915, #2993 ) ;
#6252 = DIRECTION ( 'NONE',  ( -0.000000000000000000, -0.000000000000000000, -1.000000000000000000 ) ) ;
#6253 = EDGE_CURVE ( 'NONE', #1907, #3857, #273, .T. ) ;
#6254 = CYLINDRICAL_SURFACE ( 'NONE', #6545, 40.00000000000000711 ) ;
#6255 = DIRECTION ( 'NONE',  ( 0.000000000000000000, 0.000000000000000000, -1.000000000000000000 ) ) ;
#6256 = PRODUCT_CONTEXT ( 'NONE', #6915, 'mechanical' ) ;
#6257 = AXIS2_PLACEMENT_3D ( 'NONE', #2032, #6874, #6913 ) ;
#6258 = EDGE_CURVE ( 'NONE', #4189, #589, #1157, .T. ) ;
#6259 = CARTESIAN_POINT ( 'NONE',  ( 4.000000000000005329, -6.928203230275506108, -4.700000000000000178 ) ) ;
#6260 = DIRECTION ( 'NONE',  ( -0.000000000000000000, -0.000000000000000000, 1.000000000000000000 ) ) ;
#6261 = ORIENTED_EDGE ( 'NONE', *, *, #4278, .F. ) ;
#6262 = ORIENTED_EDGE ( 'NONE', *, *, #5047, .F. ) ;
#6263 = ORIENTED_EDGE ( 'NONE', *, *, #5394, .F. ) ;
#6264 = EDGE_CURVE ( 'NONE', #1121, #6339, #6202, .T. ) ;
#6265 = CIRCLE ( 'NONE', #462, 5.000000000000000888 ) ;
#6266 = ORIENTED_EDGE ( 'NONE', *, *, #6610, .T. ) ;
#6267 = CARTESIAN_POINT ( 'NONE',  ( -8.000000000000000000, -4.618802153517012954, -4.700000000000000178 ) ) ;
#6268 = CARTESIAN_POINT ( 'NONE',  ( -8.000000000000000000, 0.7809653281576030004, 7.623296525288699970E-18 ) ) ;
#6269 = DIRECTION ( 'NONE',  ( -1.000000000000000000, 0.000000000000000000, 0.000000000000000000 ) ) ;
#6270 = EDGE_CURVE ( 'NONE', #5391, #5644, #153, .T. ) ;
#6271 = AXIS2_PLACEMENT_3D ( 'NONE', #6775, #5466, #770 ) ;
#6272 = ORIENTED_EDGE ( 'NONE', *, *, #3694, .T. ) ;
#6273 = ORIENTED_EDGE ( 'NONE', *, *, #803, .T. ) ;
#6274 = AXIS2_PLACEMENT_3D ( 'NONE', #5815, #5263, #7625 ) ;
#6275 = DIRECTION ( 'NONE',  ( -0.000000000000000000, -0.000000000000000000, 1.000000000000000000 ) ) ;
#6276 =( LENGTH_UNIT ( ) NAMED_UNIT ( * ) SI_UNIT ( .MILLI., .METRE. ) );
#6277 = CARTESIAN_POINT ( 'NONE',  ( 0.000000000000000000, 0.000000000000000000, 0.000000000000000000 ) ) ;
#6278 = CARTESIAN_POINT ( 'NONE',  ( 39.64284999284935651, 144.6666666666667140, 10.00000000000000000 ) ) ;
#6279 = DIRECTION ( 'NONE',  ( 0.9477696887085605981, 0.3189555096957539804, 1.755346904044972688E-17 ) ) ;
#6280 = ORIENTED_EDGE ( 'NONE', *, *, #1531, .F. ) ;
#6281 = AXIS2_PLACEMENT_3D ( 'NONE', #5563, #750, #2253 ) ;
#6282 = CIRCLE ( 'NONE', #978, 37.19999999999999574 ) ;
#6283 = CARTESIAN_POINT ( 'NONE',  ( 279.9963296805736945, -6.714540835673234486E-12, -50.00000000000004263 ) ) ;
#6284 = CARTESIAN_POINT ( 'NONE',  ( 37.49999999999997868, 0.000000000000000000, -90.00000000000000000 ) ) ;
#6285 = DIRECTION ( 'NONE',  ( -0.000000000000000000, -0.000000000000000000, 1.000000000000000000 ) ) ;
#6286 = DIRECTION ( 'NONE',  ( 0.000000000000000000, 0.000000000000000000, -1.000000000000000000 ) ) ;
#6287 = ORIENTED_EDGE ( 'NONE', *, *, #1240, .T. ) ;
#6288 = VECTOR ( 'NONE', #957, 1000.000000000000000 ) ;
#6289 = CARTESIAN_POINT ( 'NONE',  ( -10.00000000000000000, 0.000000000000000000, -50.00000000000000000 ) ) ;
#6290 = CARTESIAN_POINT ( 'NONE',  ( -129.9038105676655164, -75.00000000000063949, 10.00000000000000000 ) ) ;
#6291 = VECTOR ( 'NONE', #2601, 1000.000000000000000 ) ;
#6292 = LINE ( 'NONE', #6998, #6981 ) ;
#6293 = CYLINDRICAL_SURFACE ( 'NONE', #1364, 32.49999999999997158 ) ;
#6294 = DIRECTION ( 'NONE',  ( 1.000000000000000000, 0.000000000000000000, 0.000000000000000000 ) ) ;
#6295 = APPLICATION_PROTOCOL_DEFINITION ( 'draft international standard', 'automotive_design', 1998, #6213 ) ;
#6296 = CARTESIAN_POINT ( 'NONE',  ( 10.00000000000000000, 41.99999999999999289, 10.00000000000000000 ) ) ;
#6297 = EDGE_CURVE ( 'NONE', #2865, #5930, #1997, .T. ) ;
#6298 = ORIENTED_EDGE ( 'NONE', *, *, #4758, .T. ) ;
#6299 = ORIENTED_EDGE ( 'NONE', *, *, #6595, .F. ) ;
#6300 = EDGE_CURVE ( 'NONE', #5243, #7510, #392, .T. ) ;
#6301 = ORIENTED_EDGE ( 'NONE', *, *, #7355, .F. ) ;
#6302 = AXIS2_PLACEMENT_3D ( 'NONE', #5787, #7557, #4448 ) ;
#6303 = EDGE_CURVE ( 'NONE', #6148, #544, #7340, .T. ) ;
#6304 = VERTEX_POINT ( 'NONE', #3915 ) ;
#6305 = EDGE_CURVE ( 'NONE', #1335, #6520, #6175, .T. ) ;
#6306 = ORIENTED_EDGE ( 'NONE', *, *, #3368, .F. ) ;
#6307 = VECTOR ( 'NONE', #6179, 1000.000000000000000 ) ;
#6308 = CARTESIAN_POINT ( 'NONE',  ( -30.00000000000000711, 3.673940397442059967E-15, 20.00000000000000000 ) ) ;
#6309 = CARTESIAN_POINT ( 'NONE',  ( 0.000000000000000000, 0.000000000000000000, 10.00000000000000000 ) ) ;
#6310 = AXIS2_PLACEMENT_3D ( 'NONE', #1663, #4776, #4061 ) ;
#6311 = DIRECTION ( 'NONE',  ( -0.000000000000000000, -0.000000000000000000, -1.000000000000000000 ) ) ;
#6312 = EDGE_CURVE ( 'NONE', #1789, #6313, #5061, .T. ) ;
#6313 = VERTEX_POINT ( 'NONE', #2623 ) ;
#6314 = ORIENTED_EDGE ( 'NONE', *, *, #6597, .F. ) ;
#6315 = AXIS2_PLACEMENT_3D ( 'NONE', #5953, #1697, #1096 ) ;
#6316 = ORIENTED_EDGE ( 'NONE', *, *, #2264, .F. ) ;
#6317 = DIRECTION ( 'NONE',  ( -0.000000000000000000, -0.000000000000000000, 1.000000000000000000 ) ) ;
#6318 = DIRECTION ( 'NONE',  ( 0.000000000000000000, -1.000000000000000000, 0.000000000000000000 ) ) ;
#6319 = AXIS2_PLACEMENT_3D ( 'NONE', #3194, #2641, #5596 ) ;
#6320 =( REPRESENTATION_RELATIONSHIP ('NONE','NONE', #1229, #1433 ) REPRESENTATION_RELATIONSHIP_WITH_TRANSFORMATION ( #2280 )SHAPE_REPRESENTATION_RELATIONSHIP( ) );
#6321 = FACE_OUTER_BOUND ( 'NONE', #1275, .T. ) ;
#6322 = ORIENTED_EDGE ( 'NONE', *, *, #6887, .T. ) ;
#6323 = CYLINDRICAL_SURFACE ( 'NONE', #2726, 37.49999999999997868 ) ;
#6324 = CARTESIAN_POINT ( 'NONE',  ( -5.857142857142856762, 7.172931252148783106E-16, 2.573333333332999739 ) ) ;
#6325 = DIRECTION ( 'NONE',  ( 1.000000000000000000, 0.000000000000000000, 0.000000000000000000 ) ) ;
#6326 = CARTESIAN_POINT ( 'NONE',  ( 207.8429183184021269, 119.9981648402868331, -120.0000000000000000 ) ) ;
#6327 = ORIENTED_EDGE ( 'NONE', *, *, #6649, .F. ) ;
#6328 = ADVANCED_BREP_SHAPE_REPRESENTATION ( '', ( #475, #7485 ), #6367 ) ;
#6329 = DIRECTION ( 'NONE',  ( 0.000000000000000000, 0.000000000000000000, -1.000000000000000000 ) ) ;
#6330 = LINE ( 'NONE', #6955, #4099 ) ;
#6331 = DIRECTION ( 'NONE',  ( -1.000000000000000000, 0.000000000000000000, 0.000000000000000000 ) ) ;
#6332 = CARTESIAN_POINT ( 'NONE',  ( -68.76644452187068168, 49.96174644486002592, 10.00000000000000000 ) ) ;
#6333 = CARTESIAN_POINT ( 'NONE',  ( -3.199999999999996181, 4.555686092828153507E-15, 37.19999999999999574 ) ) ;
#6334 = CARTESIAN_POINT ( 'NONE',  ( -4.494751301858288528, -36.47409643479112162, 0.000000000000000000 ) ) ;
#6335 = FILL_AREA_STYLE_COLOUR ( '', #7241 ) ;
#6336 = EDGE_LOOP ( 'NONE', ( #5484, #1825, #510, #6150 ) ) ;
#6337 = ORIENTED_EDGE ( 'NONE', *, *, #6312, .T. ) ;
#6338 = CIRCLE ( 'NONE', #4940, 30.00000000000000355 ) ;
#6339 = VERTEX_POINT ( 'NONE', #5056 ) ;
#6340 = VERTEX_POINT ( 'NONE', #5022 ) ;
#6341 = CARTESIAN_POINT ( 'NONE',  ( 0.000000000000000000, 0.000000000000000000, -139.9999999999999716 ) ) ;
#6342 = DIRECTION ( 'NONE',  ( 1.000000000000000000, 0.000000000000000000, 0.000000000000000000 ) ) ;
#6343 = CARTESIAN_POINT ( 'NONE',  ( -68.76644452187068168, 49.96174644486002592, -40.00000000000000000 ) ) ;
#6344 = CARTESIAN_POINT ( 'NONE',  ( 0.000000000000000000, 0.000000000000000000, 0.000000000000000000 ) ) ;
#6345 = CARTESIAN_POINT ( 'NONE',  ( 0.000000000000000000, 0.000000000000000000, 10.00000000000000000 ) ) ;
#6346 = EDGE_CURVE ( 'NONE', #6348, #2067, #3843, .T. ) ;
#6347 = EDGE_LOOP ( 'NONE', ( #5266, #3820, #2282, #1454 ) ) ;
#6348 = VERTEX_POINT ( 'NONE', #1508 ) ;
#6349 = AXIS2_PLACEMENT_3D ( 'NONE', #1017, #6432, #7099 ) ;
#6350 = ORIENTED_EDGE ( 'NONE', *, *, #2069, .T. ) ;
#6351 = CARTESIAN_POINT ( 'NONE',  ( -78.76644452187068168, 49.96174644486002592, -40.00000000000000000 ) ) ;
#6352 = ADVANCED_FACE ( 'NONE', ( #279 ), #2036, .T. ) ;
#6353 = DIRECTION ( 'NONE',  ( 1.000000000000000000, 0.000000000000000000, 0.000000000000000000 ) ) ;
#6354 = AXIS2_PLACEMENT_3D ( 'NONE', #7010, #6501, #5869 ) ;
#6355 = AXIS2_PLACEMENT_3D ( 'NONE', #7461, #2071, #5763 ) ;
#6356 = LINE ( 'NONE', #7648, #4443 ) ;
#6357 = VERTEX_POINT ( 'NONE', #1957 ) ;
#6358 =( GEOMETRIC_REPRESENTATION_CONTEXT ( 3 ) GLOBAL_UNCERTAINTY_ASSIGNED_CONTEXT ( ( #7318 ) ) GLOBAL_UNIT_ASSIGNED_CONTEXT ( ( #4479, #6892, #6815 ) ) REPRESENTATION_CONTEXT ( 'NONE', 'WORKASPACE' ) );
#6359 = EDGE_CURVE ( 'NONE', #1025, #1930, #4309, .T. ) ;
#6360 =( GEOMETRIC_REPRESENTATION_CONTEXT ( 3 ) GLOBAL_UNCERTAINTY_ASSIGNED_CONTEXT ( ( #7288 ) ) GLOBAL_UNIT_ASSIGNED_CONTEXT ( ( #3548, #4053, #2223 ) ) REPRESENTATION_CONTEXT ( 'NONE', 'WORKASPACE' ) );
#6361 = DIRECTION ( 'NONE',  ( 0.000000000000000000, 0.000000000000000000, 1.000000000000000000 ) ) ;
#6362 = CARTESIAN_POINT ( 'NONE',  ( -58.76644452187068168, 49.96174644486002592, 0.000000000000000000 ) ) ;
#6363 = CARTESIAN_POINT ( 'NONE',  ( -63.51644452187067458, 49.96174644486002592, 0.000000000000000000 ) ) ;
#6364 = CARTESIAN_POINT ( 'NONE',  ( -4.000000000000004441, -6.928203230275506108, -4.700000000000000178 ) ) ;
#6365 = EDGE_CURVE ( 'NONE', #544, #6903, #171, .T. ) ;
#6366 = ORIENTED_EDGE ( 'NONE', *, *, #5528, .F. ) ;
#6367 =( GEOMETRIC_REPRESENTATION_CONTEXT ( 3 ) GLOBAL_UNCERTAINTY_ASSIGNED_CONTEXT ( ( #7387 ) ) GLOBAL_UNIT_ASSIGNED_CONTEXT ( ( #1979, #4369, #6152 ) ) REPRESENTATION_CONTEXT ( 'NONE', 'WORKASPACE' ) );
#6368 = CARTESIAN_POINT ( 'NONE',  ( 350.0000000000000000, -300.0000000000000000, -120.0000000000000000 ) ) ;
#6369 = CYLINDRICAL_SURFACE ( 'NONE', #2851, 40.00000000000000711 ) ;
#6370 = CARTESIAN_POINT ( 'NONE',  ( 0.000000000000000000, 0.000000000000000000, 10.00000000000000000 ) ) ;
#6371 = DIRECTION ( 'NONE',  ( 1.000000000000000000, 0.000000000000000000, 0.000000000000000000 ) ) ;
#6372 = CARTESIAN_POINT ( 'NONE',  ( 2.583028308771596837, 28.38270538120150377, 13.00000000000000178 ) ) ;
#6373 = ITEM_DEFINED_TRANSFORMATION ( 'NONE', 'NONE', #5610,  #7485 ) ;
#6374 = DIRECTION ( 'NONE',  ( 0.9938725510941108787, -0.1105321318969463978, 0.000000000000000000 ) ) ;
#6375 = VERTEX_POINT ( 'NONE', #5688 ) ;
#6376 = COLOUR_RGB ( '',0.8941176470588234615, 0.8941176470588234615, 0.8941176470588234615 ) ;
#6377 = EDGE_LOOP ( 'NONE', ( #2800, #4974, #2588, #5474 ) ) ;
#6378 = ORIENTED_EDGE ( 'NONE', *, *, #1668, .F. ) ;
#6379 = ORIENTED_EDGE ( 'NONE', *, *, #3927, .T. ) ;
#6380 = DIRECTION ( 'NONE',  ( 0.000000000000000000, 0.000000000000000000, 1.000000000000000000 ) ) ;
#6381 = CIRCLE ( 'NONE', #1855, 199.9963296805737230 ) ;
#6382 = CARTESIAN_POINT ( 'NONE',  ( 7.347286611336969031, 4.995646404165278831, -0.4969600502617517734 ) ) ;
#6383 = CARTESIAN_POINT ( 'NONE',  ( -8.000000000000000000, 0.000000000000000000, 0.000000000000000000 ) ) ;
#6384 = DIRECTION ( 'NONE',  ( -1.000000000000000000, 0.000000000000000000, 0.000000000000000000 ) ) ;
#6385 = EDGE_CURVE ( 'NONE', #4712, #5807, #31, .T. ) ;
#6386 = EDGE_LOOP ( 'NONE', ( #7080, #1327, #561, #350 ) ) ;
#6387 = AXIS2_PLACEMENT_3D ( 'NONE', #2771, #2810, #2266 ) ;
#6388 = ORIENTED_EDGE ( 'NONE', *, *, #4552, .F. ) ;
#6389 = ORIENTED_EDGE ( 'NONE', *, *, #6878, .T. ) ;
#6390 = PLANE ( 'NONE',  #6435 ) ;
#6391 = PRESENTATION_STYLE_ASSIGNMENT (( #7685 ) ) ;
#6392 = VECTOR ( 'NONE', #692, 1000.000000000000000 ) ;
#6393 = DIRECTION ( 'NONE',  ( -0.000000000000000000, -0.000000000000000000, 1.000000000000000000 ) ) ;
#6394 = CARTESIAN_POINT ( 'NONE',  ( -9.702951051037022268, -29.86427928513813512, 0.000000000000000000 ) ) ;
#6395 = EDGE_CURVE ( 'NONE', #3123, #2201, #1392, .T. ) ;
#6396 = ORIENTED_EDGE ( 'NONE', *, *, #2548, .T. ) ;
#6397 = EDGE_CURVE ( 'NONE', #5742, #5317, #243, .T. ) ;
#6398 = EDGE_CURVE ( 'NONE', #2609, #738, #3928, .T. ) ;
#6399 = AXIS2_PLACEMENT_3D ( 'NONE', #5979, #4668, #7075 ) ;
#6400 = EDGE_CURVE ( 'NONE', #7233, #6357, #6835, .T. ) ;
#6401 = CARTESIAN_POINT ( 'NONE',  ( 0.000000000000000000, 0.000000000000000000, 10.00000000000000000 ) ) ;
#6402 = DIRECTION ( 'NONE',  ( 1.000000000000000000, 0.000000000000000000, 0.000000000000000000 ) ) ;
#6403 = CARTESIAN_POINT ( 'NONE',  ( 10.16320117273318679, -26.62629042736811869, -122.9999999999999716 ) ) ;
#6404 = LINE ( 'NONE', #2311, #6453 ) ;
#6405 = EDGE_LOOP ( 'NONE', ( #4553, #4291 ) ) ;
#6406 = EDGE_CURVE ( 'NONE', #4996, #2067, #3428, .T. ) ;
#6407 = EDGE_CURVE ( 'NONE', #5930, #1219, #4434, .T. ) ;
#6408 = CARTESIAN_POINT ( 'NONE',  ( 0.000000000000000000, 0.000000000000000000, 19.04999999999997229 ) ) ;
#6409 = VECTOR ( 'NONE', #3281, 1000.000000000000000 ) ;
#6410 = CARTESIAN_POINT ( 'NONE',  ( 35.00000000000000711, 4.286263797015737285E-15, -50.00000000000000000 ) ) ;
#6411 = DIRECTION ( 'NONE',  ( -0.000000000000000000, -0.000000000000000000, 1.000000000000000000 ) ) ;
#6412 = DIRECTION ( 'NONE',  ( -0.000000000000000000, -0.000000000000000000, -1.000000000000000000 ) ) ;
#6413 = FACE_OUTER_BOUND ( 'NONE', #1779, .T. ) ;
#6414 = CIRCLE ( 'NONE', #6041, 32.49999999999997158 ) ;
#6415 = CARTESIAN_POINT ( 'NONE',  ( 3.200000000000008171, 3.692310099429270397E-15, 30.00000000000000000 ) ) ;
#6416 = ORIENTED_EDGE ( 'NONE', *, *, #4853, .F. ) ;
#6417 = ORIENTED_EDGE ( 'NONE', *, *, #6944, .F. ) ;
#6418 = ORIENTED_EDGE ( 'NONE', *, *, #6062, .F. ) ;
#6419 = CIRCLE ( 'NONE', #1503, 150.0000000000000568 ) ;
#6420 = CARTESIAN_POINT ( 'NONE',  ( -4.000000000000004441, 6.928203230275506108, -4.700000000000000178 ) ) ;
#6421 =( REPRESENTATION_RELATIONSHIP ('NONE','NONE', #1229, #2561 ) REPRESENTATION_RELATIONSHIP_WITH_TRANSFORMATION ( #4633 )SHAPE_REPRESENTATION_RELATIONSHIP( ) );
#6422 = CARTESIAN_POINT ( 'NONE',  ( -29.99999999999999289, 3.673940397442058389E-15, -139.9999999999999716 ) ) ;
#6423 = CARTESIAN_POINT ( 'NONE',  ( 207.8429183184020985, 119.9981648402868331, 10.00000000000000178 ) ) ;
#6424 = CARTESIAN_POINT ( 'NONE',  ( 0.000000000000000000, 0.000000000000000000, 0.000000000000000000 ) ) ;
#6425 =( NAMED_UNIT ( * ) PLANE_ANGLE_UNIT ( ) SI_UNIT ( $, .RADIAN. ) );
#6426 = CARTESIAN_POINT ( 'NONE',  ( 119.9981648402868899, 207.8429183184021269, -8.673617379884035472E-15 ) ) ;
#6427 = VERTEX_POINT ( 'NONE', #3768 ) ;
#6428 = EDGE_LOOP ( 'NONE', ( #6366, #624, #1110, #1639 ) ) ;
#6429 = ORIENTED_EDGE ( 'NONE', *, *, #5481, .T. ) ;
#6430 = CIRCLE ( 'NONE', #5669, 5.249999999999997335 ) ;
#6431 = CARTESIAN_POINT ( 'NONE',  ( -199.9963296805737230, 0.000000000000000000, 10.00000000000000000 ) ) ;
#6432 = DIRECTION ( 'NONE',  ( 0.000000000000000000, 0.000000000000000000, -1.000000000000000000 ) ) ;
#6433 = DIRECTION ( 'NONE',  ( -0.000000000000000000, 1.000000000000000000, 0.000000000000000000 ) ) ;
#6434 = VERTEX_POINT ( 'NONE', #7656 ) ;
#6435 = AXIS2_PLACEMENT_3D ( 'NONE', #7526, #1497, #861 ) ;
#6436 = CARTESIAN_POINT ( 'NONE',  ( 0.000000000000000000, 0.000000000000000000, -112.9999999999999716 ) ) ;
#6437 = CARTESIAN_POINT ( 'NONE',  ( -125.2481648402867762, 207.8429183184021554, 10.00000000000000178 ) ) ;
#6438 = VECTOR ( 'NONE', #4252, 1000.000000000000000 ) ;
#6439 = DIRECTION ( 'NONE',  ( 1.000000000000000000, 0.000000000000000000, 0.000000000000000000 ) ) ;
#6440 = DIRECTION ( 'NONE',  ( -0.000000000000000000, -0.000000000000000000, 1.000000000000000000 ) ) ;
#6441 = ORIENTED_EDGE ( 'NONE', *, *, #4820, .T. ) ;
#6442 = EDGE_CURVE ( 'NONE', #4594, #4452, #5447, .T. ) ;
#6443 = ORIENTED_EDGE ( 'NONE', *, *, #5427, .T. ) ;
#6444 = CARTESIAN_POINT ( 'NONE',  ( 0.5700000000000001732, -28.49429942988597020, 0.000000000000000000 ) ) ;
#6445 = DIRECTION ( 'NONE',  ( -0.000000000000000000, 1.000000000000000000, 0.000000000000000000 ) ) ;
#6446 = CARTESIAN_POINT ( 'NONE',  ( -199.9963296805737230, 2.449248649845333917E-14, 576.0908266162076643 ) ) ;
#6447 = CARTESIAN_POINT ( 'NONE',  ( 202.5929183184021554, 119.9981648402868331, -120.0000000000000000 ) ) ;
#6448 = ADVANCED_FACE ( 'NONE', ( #951 ), #4064, .F. ) ;
#6449 = DIRECTION ( 'NONE',  ( -1.000000000000000000, 0.000000000000000000, 0.000000000000000000 ) ) ;
#6450 = VERTEX_POINT ( 'NONE', #2894 ) ;
#6451 = ORIENTED_EDGE ( 'NONE', *, *, #223, .T. ) ;
#6452 = ORIENTED_EDGE ( 'NONE', *, *, #6160, .F. ) ;
#6453 = VECTOR ( 'NONE', #2233, 1000.000000000000000 ) ;
#6454 = CARTESIAN_POINT ( 'NONE',  ( -3.660532965668821248, 7.124194613927619102, -4.700000000000004619 ) ) ;
#6455 = DIRECTION ( 'NONE',  ( -0.000000000000000000, -0.000000000000000000, -1.000000000000000000 ) ) ;
#6456 = CARTESIAN_POINT ( 'NONE',  ( -29.99999999999999289, 3.673940397442058389E-15, -139.9999999999999716 ) ) ;
#6457 = DIRECTION ( 'NONE',  ( 1.000000000000000000, 0.000000000000000000, 0.000000000000000000 ) ) ;
#6458 = CIRCLE ( 'NONE', #1411, 5.249999999999988454 ) ;
#6459 = EDGE_CURVE ( 'NONE', #3615, #387, #1588, .T. ) ;
#6460 = EDGE_LOOP ( 'NONE', ( #3607, #7486, #7012, #4701 ) ) ;
#6461 = ORIENTED_EDGE ( 'NONE', *, *, #2838, .T. ) ;
#6462 = ORIENTED_EDGE ( 'NONE', *, *, #268, .T. ) ;
#6463 = CIRCLE ( 'NONE', #5075, 30.00000000000000000 ) ;
#6464 = DIRECTION ( 'NONE',  ( 0.9938725510941108787, -0.1105321318969463978, 0.000000000000000000 ) ) ;
#6465 = DIRECTION ( 'NONE',  ( 0.000000000000000000, 0.000000000000000000, 1.000000000000000000 ) ) ;
#6466 =( NAMED_UNIT ( * ) SI_UNIT ( $, .STERADIAN. ) SOLID_ANGLE_UNIT ( ) );
#6467 = CARTESIAN_POINT ( 'NONE',  ( 0.000000000000000000, 0.000000000000000000, -122.9999999999999716 ) ) ;
#6468 = DIRECTION ( 'NONE',  ( 0.000000000000000000, 0.000000000000000000, 1.000000000000000000 ) ) ;
#6469 = CIRCLE ( 'NONE', #3828, 4.999999999999990230 ) ;
#6470 = EDGE_LOOP ( 'NONE', ( #5006, #7438 ) ) ;
#6471 = DIRECTION ( 'NONE',  ( 0.000000000000000000, 0.000000000000000000, -1.000000000000000000 ) ) ;
#6472 = DIRECTION ( 'NONE',  ( -1.000000000000000000, 0.000000000000000000, 0.000000000000000000 ) ) ;
#6473 = CIRCLE ( 'NONE', #4966, 35.00000000000000711 ) ;
#6474 = VECTOR ( 'NONE', #1422, 1000.000000000000000 ) ;
#6475 = FACE_OUTER_BOUND ( 'NONE', #3397, .T. ) ;
#6476 = DIRECTION ( 'NONE',  ( -0.000000000000000000, -0.000000000000000000, 1.000000000000000000 ) ) ;
#6477 = ORIENTED_EDGE ( 'NONE', *, *, #1290, .T. ) ;
#6478 = PRODUCT_DEFINITION ( 'UNKNOWN', '', #783, #4059 ) ;
#6479 = ORIENTED_EDGE ( 'NONE', *, *, #5568, .F. ) ;
#6480 = PRESENTATION_LAYER_ASSIGNMENT (  '', '', ( #3836 ) ) ;
#6481 = STYLED_ITEM ( 'NONE', ( #5299 ), #5187 ) ;
#6482 = CARTESIAN_POINT ( 'NONE',  ( -39.64284999284934230, 144.6666666666667140, 0.000000000000000000 ) ) ;
#6483 = CARTESIAN_POINT ( 'NONE',  ( -20.63749999999999929, 0.000000000000000000, -31.52499999999999858 ) ) ;
#6484 = CARTESIAN_POINT ( 'NONE',  ( 3.716043017018883621, 28.25669875083898930, 13.00000000000000178 ) ) ;
#6485 = CARTESIAN_POINT ( 'NONE',  ( -68.76644452187072432, 49.96174644486006855, -40.00000000000000000 ) ) ;
#6486 = DIRECTION ( 'NONE',  ( 0.000000000000000000, 0.000000000000000000, 1.000000000000000000 ) ) ;
#6487 =( GEOMETRIC_REPRESENTATION_CONTEXT ( 3 ) GLOBAL_UNCERTAINTY_ASSIGNED_CONTEXT ( ( #1374 ) ) GLOBAL_UNIT_ASSIGNED_CONTEXT ( ( #4771, #1858, #6744 ) ) REPRESENTATION_CONTEXT ( 'NONE', 'WORKASPACE' ) );
#6488 = DIRECTION ( 'NONE',  ( -0.000000000000000000, -0.000000000000000000, 1.000000000000000000 ) ) ;
#6489 = ORIENTED_EDGE ( 'NONE', *, *, #7499, .F. ) ;
#6490 = EDGE_CURVE ( 'NONE', #5377, #7515, #6404, .T. ) ;
#6491 = ORIENTED_EDGE ( 'NONE', *, *, #4024, .F. ) ;
#6492 = VERTEX_POINT ( 'NONE', #359 ) ;
#6493 = EDGE_CURVE ( 'NONE', #4251, #4674, #7458, .T. ) ;
#6494 = ADVANCED_FACE ( 'NONE', ( #1069 ), #1547, .F. ) ;
#6495 = DIRECTION ( 'NONE',  ( 0.9938725510941108787, -0.1105321318969463978, 0.000000000000000000 ) ) ;
#6496 = EDGE_CURVE ( 'NONE', #3054, #2582, #593, .T. ) ;
#6497 = DIRECTION ( 'NONE',  ( 0.7071067811865474617, 0.000000000000000000, 0.7071067811865474617 ) ) ;
#6498 = CARTESIAN_POINT ( 'NONE',  ( 0.000000000000000000, -150.0000000000000568, 10.00000000000000000 ) ) ;
#6499 = SURFACE_SIDE_STYLE ('',( #3386 ) ) ;
#6500 = CIRCLE ( 'NONE', #3976, 150.0000000000000568 ) ;
#6501 = DIRECTION ( 'NONE',  ( -5.635681009894454322E-17, -1.505185443864239327E-19, -1.000000000000000000 ) ) ;
#6502 = PLANE ( 'NONE',  #4 ) ;
#6503 = ORIENTED_EDGE ( 'NONE', *, *, #1138, .F. ) ;
#6504 = EDGE_CURVE ( 'NONE', #1573, #2088, #7107, .T. ) ;
#6505 = ORIENTED_EDGE ( 'NONE', *, *, #4020, .F. ) ;
#6506 = EDGE_LOOP ( 'NONE', ( #2828, #5023, #4337, #5629 ) ) ;
#6507 = FACE_OUTER_BOUND ( 'NONE', #5711, .T. ) ;
#6508 = DIRECTION ( 'NONE',  ( 0.000000000000000000, 0.000000000000000000, -1.000000000000000000 ) ) ;
#6509 = ADVANCED_FACE ( 'NONE', ( #7536 ), #4104, .T. ) ;
#6510 = CARTESIAN_POINT ( 'NONE',  ( -20.63749999999999929, 0.000000000000000000, 0.000000000000000000 ) ) ;
#6511 = CIRCLE ( 'NONE', #3986, 28.50000000000000711 ) ;
#6512 = FACE_OUTER_BOUND ( 'NONE', #1998, .T. ) ;
#6513 = ORIENTED_EDGE ( 'NONE', *, *, #4613, .T. ) ;
#6514 = UNCERTAINTY_MEASURE_WITH_UNIT (LENGTH_MEASURE( 1.000000000000000082E-05 ), #1933, 'distance_accuracy_value', 'NONE');
#6515 = AXIS2_PLACEMENT_3D ( 'NONE', #5867, #1047, #5944 ) ;
#6516 = DIRECTION ( 'NONE',  ( 3.081487911019577365E-33, -2.775557561562891967E-17, -1.000000000000000000 ) ) ;
#6517 = DIRECTION ( 'NONE',  ( -0.000000000000000000, -0.000000000000000000, 1.000000000000000000 ) ) ;
#6518 = LINE ( 'NONE', #2232, #2000 ) ;
#6519 = CARTESIAN_POINT ( 'NONE',  ( -6.689127551062008514, -5.375634714784628621, -4.382649155111343120 ) ) ;
#6520 = VERTEX_POINT ( 'NONE', #2190 ) ;
#6521 = AXIS2_PLACEMENT_3D ( 'NONE', #4949, #1964, #1848 ) ;
#6522 = ORIENTED_EDGE ( 'NONE', *, *, #6127, .F. ) ;
#6523 = DIRECTION ( 'NONE',  ( -0.000000000000000000, -0.000000000000000000, 1.000000000000000000 ) ) ;
#6524 = CARTESIAN_POINT ( 'NONE',  ( -68.76644452187068168, 49.96174644486002592, -64.17200000000001125 ) ) ;
#6525 = CIRCLE ( 'NONE', #1996, 37.19999999999999574 ) ;
#6526 = CARTESIAN_POINT ( 'NONE',  ( -8.000000000000001776, -3.867591403079179813, -4.202324684675414979 ) ) ;
#6527 = DIRECTION ( 'NONE',  ( 1.000000000000000000, 0.000000000000000000, 0.000000000000000000 ) ) ;
#6528 = DIRECTION ( 'NONE',  ( 0.1948910352220799280, -0.9808248999643441879, -1.110223024625155793E-18 ) ) ;
#6529 = CYLINDRICAL_SURFACE ( 'NONE', #4470, 4.999999999999990230 ) ;
#6530 = PRODUCT_DEFINITION_CONTEXT ( 'detailed design', #2795, 'design' ) ;
#6531 = EDGE_LOOP ( 'NONE', ( #4520, #6020, #4927, #4289 ) ) ;
#6532 = VERTEX_POINT ( 'NONE', #1108 ) ;
#6533 = AXIS2_PLACEMENT_3D ( 'NONE', #2852, #7697, #6439 ) ;
#6534 = ORIENTED_EDGE ( 'NONE', *, *, #2115, .T. ) ;
#6535 = CARTESIAN_POINT ( 'NONE',  ( -7.345652830558760726, 4.996589667937370471, -0.4964154566687939973 ) ) ;
#6536 = VECTOR ( 'NONE', #3186, 1000.000000000000000 ) ;
#6537 = ADVANCED_FACE ( 'NONE', ( #4624 ), #3404, .T. ) ;
#6538 = FACE_OUTER_BOUND ( 'NONE', #1211, .T. ) ;
#6539 = CARTESIAN_POINT ( 'NONE',  ( 207.8429183184020985, 119.9981648402868331, 10.00000000000000000 ) ) ;
#6540 = DIRECTION ( 'NONE',  ( 3.926253788359943074E-17, 3.101873702526142631E-17, -0.9999999999999998890 ) ) ;
#6541 = DIRECTION ( 'NONE',  ( 1.000000000000000000, 0.000000000000000000, 0.000000000000000000 ) ) ;
#6542 = EDGE_CURVE ( 'NONE', #2537, #3123, #4582, .T. ) ;
#6543 = ADVANCED_FACE ( 'NONE', ( #6951 ), #3308, .F. ) ;
#6544 = ORIENTED_EDGE ( 'NONE', *, *, #1443, .T. ) ;
#6545 = AXIS2_PLACEMENT_3D ( 'NONE', #7360, #3256, #248 ) ;
#6546 = ADVANCED_FACE ( 'NONE', ( #2814 ), #2853, .F. ) ;
#6547 = ORIENTED_EDGE ( 'NONE', *, *, #6025, .T. ) ;
#6548 = ORIENTED_EDGE ( 'NONE', *, *, #2115, .F. ) ;
#6549 = DIRECTION ( 'NONE',  ( -0.000000000000000000, -0.000000000000000000, 1.000000000000000000 ) ) ;
#6550 = DIRECTION ( 'NONE',  ( 1.000000000000000000, 0.000000000000000000, 0.000000000000000000 ) ) ;
#6551 = AXIS2_PLACEMENT_3D ( 'NONE', #5660, #4134, #7216 ) ;
#6552 = CARTESIAN_POINT ( 'NONE',  ( 35.00000000000000711, 4.286263797015737285E-15, -60.00000000000000711 ) ) ;
#6553 = EDGE_CURVE ( 'NONE', #6807, #6712, #5320, .T. ) ;
#6554 = ORIENTED_EDGE ( 'NONE', *, *, #3571, .T. ) ;
#6555 = VECTOR ( 'NONE', #4101, 1000.000000000000000 ) ;
#6556 = DIRECTION ( 'NONE',  ( 0.000000000000000000, -1.000000000000000000, 0.000000000000000000 ) ) ;
#6557 = LINE ( 'NONE', #3435, #6555 ) ;
#6558 = DIRECTION ( 'NONE',  ( -1.000000000000000000, 0.000000000000000000, 0.000000000000000000 ) ) ;
#6559 = AXIS2_PLACEMENT_3D ( 'NONE', #3353, #2650, #7488 ) ;
#6560 = FACE_OUTER_BOUND ( 'NONE', #3904, .T. ) ;
#6561 = EDGE_LOOP ( 'NONE', ( #4491, #2896, #6562, #2229 ) ) ;
#6562 = ORIENTED_EDGE ( 'NONE', *, *, #1375, .T. ) ;
#6563 = VERTEX_POINT ( 'NONE', #4662 ) ;
#6564 = VECTOR ( 'NONE', #4016, 1000.000000000000000 ) ;
#6565 = DIRECTION ( 'NONE',  ( 0.000000000000000000, 0.000000000000000000, -1.000000000000000000 ) ) ;
#6566 = CARTESIAN_POINT ( 'NONE',  ( -202.5929183184021269, 119.9981648402869467, -8.673617379884035472E-15 ) ) ;
#6567 = CARTESIAN_POINT ( 'NONE',  ( 8.000000000000000000, 1.572549600175618956, -0.06894455525513237815 ) ) ;
#6568 = DIRECTION ( 'NONE',  ( -0.7071067811865474617, 8.659560562354932858E-17, 0.7071067811865474617 ) ) ;
#6569 = DIRECTION ( 'NONE',  ( 1.000000000000000000, 0.000000000000000000, 0.000000000000000000 ) ) ;
#6570 = FACE_OUTER_BOUND ( 'NONE', #1725, .T. ) ;
#6571 = VERTEX_POINT ( 'NONE', #4895 ) ;
#6572 =( REPRESENTATION_RELATIONSHIP ('NONE','NONE', #1229, #7725 ) REPRESENTATION_RELATIONSHIP_WITH_TRANSFORMATION ( #3878 )SHAPE_REPRESENTATION_RELATIONSHIP( ) );
#6573 = ORIENTED_EDGE ( 'NONE', *, *, #6496, .T. ) ;
#6574 = CYLINDRICAL_SURFACE ( 'NONE', #5733, 4.999999999999990230 ) ;
#6575 = DIRECTION ( 'NONE',  ( -3.081487911019577365E-33, 2.775557561562891967E-17, 1.000000000000000000 ) ) ;
#6576 = DIRECTION ( 'NONE',  ( -0.000000000000000000, -0.000000000000000000, -1.000000000000000000 ) ) ;
#6577 = DIRECTION ( 'NONE',  ( 0.000000000000000000, 0.000000000000000000, -1.000000000000000000 ) ) ;
#6578 = DIRECTION ( 'NONE',  ( -1.000000000000000000, 0.000000000000000000, 0.000000000000000000 ) ) ;
#6579 = CARTESIAN_POINT ( 'NONE',  ( -350.0000000000000000, -299.9999999999998863, -82.99999999999998579 ) ) ;
#6580 = ORIENTED_EDGE ( 'NONE', *, *, #3793, .T. ) ;
#6581 = VECTOR ( 'NONE', #5650, 1000.000000000000000 ) ;
#6582 = ORIENTED_EDGE ( 'NONE', *, *, #1140, .T. ) ;
#6583 = EDGE_CURVE ( 'NONE', #3431, #1373, #37, .T. ) ;
#6584 = ORIENTED_EDGE ( 'NONE', *, *, #1480, .F. ) ;
#6585 = CARTESIAN_POINT ( 'NONE',  ( 0.000000000000000000, 0.000000000000000000, -4.700000000000000178 ) ) ;
#6586 = CARTESIAN_POINT ( 'NONE',  ( -8.000000000000001776, -3.867591403079177592, -0.4976753153245848660 ) ) ;
#6587 =( NAMED_UNIT ( * ) PLANE_ANGLE_UNIT ( ) SI_UNIT ( $, .RADIAN. ) );
#6588 = CIRCLE ( 'NONE', #3313, 5.250000000000004441 ) ;
#6589 = EDGE_CURVE ( 'NONE', #5633, #4160, #6674, .T. ) ;
#6590 = FACE_OUTER_BOUND ( 'NONE', #3039, .T. ) ;
#6591 = DIRECTION ( 'NONE',  ( -1.000000000000000000, 0.000000000000000000, 0.000000000000000000 ) ) ;
#6592 = EDGE_LOOP ( 'NONE', ( #6534, #4557, #4570, #1939 ) ) ;
#6593 = EDGE_LOOP ( 'NONE', ( #1833, #5277, #2801, #344 ) ) ;
#6594 = AXIS2_PLACEMENT_3D ( 'NONE', #5934, #6969, #5785 ) ;
#6595 = EDGE_CURVE ( 'NONE', #6736, #6532, #1672, .T. ) ;
#6596 = CARTESIAN_POINT ( 'NONE',  ( 32.81578194438969120, 1.484218055610305731, 0.000000000000000000 ) ) ;
#6597 = EDGE_CURVE ( 'NONE', #7617, #1428, #1031, .T. ) ;
#6598 = DIRECTION ( 'NONE',  ( 1.000000000000000000, 0.000000000000000000, 0.000000000000000000 ) ) ;
#6599 = DIRECTION ( 'NONE',  ( -1.000000000000000000, -1.776356839400250465E-15, 0.000000000000000000 ) ) ;
#6600 = ORIENTED_EDGE ( 'NONE', *, *, #7226, .T. ) ;
#6601 = ORIENTED_EDGE ( 'NONE', *, *, #2279, .F. ) ;
#6602 = EDGE_CURVE ( 'NONE', #1051, #1102, #4816, .T. ) ;
#6603 = ORIENTED_EDGE ( 'NONE', *, *, #7121, .T. ) ;
#6604 = AXIS2_PLACEMENT_3D ( 'NONE', #6345, #5040, #2097 ) ;
#6605 = CIRCLE ( 'NONE', #2580, 150.0000000000000568 ) ;
#6606 = DIRECTION ( 'NONE',  ( 0.000000000000000000, 1.224646799147359124E-16, 1.000000000000000000 ) ) ;
#6607 = CARTESIAN_POINT ( 'NONE',  ( 3.199999999999996181, 0.000000000000000000, 0.000000000000000000 ) ) ;
#6608 = DIRECTION ( 'NONE',  ( -1.000000000000000000, 1.586032892321652729E-16, 0.000000000000000000 ) ) ;
#6609 = DIRECTION ( 'NONE',  ( 0.000000000000000000, 0.000000000000000000, -1.000000000000000000 ) ) ;
#6610 = EDGE_CURVE ( 'NONE', #1102, #6304, #1162, .T. ) ;
#6611 = UNCERTAINTY_MEASURE_WITH_UNIT (LENGTH_MEASURE( 1.000000000000000082E-05 ), #1895, 'distance_accuracy_value', 'NONE');
#6612 = CARTESIAN_POINT ( 'NONE',  ( -29.99999999999999289, 3.673940397442058389E-15, -50.00000000000000000 ) ) ;
#6613 = ORIENTED_EDGE ( 'NONE', *, *, #6984, .T. ) ;
#6614 = VECTOR ( 'NONE', #2943, 1000.000000000000000 ) ;
#6615 = VERTEX_POINT ( 'NONE', #6007 ) ;
#6616 = FACE_OUTER_BOUND ( 'NONE', #1253, .T. ) ;
#6617 = CIRCLE ( 'NONE', #2091, 1.250000000000000444 ) ;
#6618 = CARTESIAN_POINT ( 'NONE',  ( -0.3344772040064616925, 0.000000000000000000, 35.97500000000000853 ) ) ;
#6619 = FACE_OUTER_BOUND ( 'NONE', #3926, .T. ) ;
#6620 = DIRECTION ( 'NONE',  ( 0.6497489119555339698, -0.7601489008165439598, 1.931932416011734352E-18 ) ) ;
#6621 = APPLICATION_CONTEXT ( 'automotive_design' ) ;
#6622 = CARTESIAN_POINT ( 'NONE',  ( -1.734723475976807094E-15, 9.237604307034017026, -3.985468820183668104 ) ) ;
#6623 = CARTESIAN_POINT ( 'NONE',  ( 202.5929183184021554, 119.9981648402868331, -50.00000000000000000 ) ) ;
#6624 = ORIENTED_EDGE ( 'NONE', *, *, #6169, .T. ) ;
#6625 = AXIS2_PLACEMENT_3D ( 'NONE', #2996, #3579, #1734 ) ;
#6626 = EDGE_LOOP ( 'NONE', ( #3276, #4635, #2304, #360 ) ) ;
#6627 = ORIENTED_EDGE ( 'NONE', *, *, #7549, .F. ) ;
#6628 = FACE_OUTER_BOUND ( 'NONE', #2570, .T. ) ;
#6629 = CARTESIAN_POINT ( 'NONE',  ( -3.499999999999996003, 0.000000000000000000, -35.97500000000000142 ) ) ;
#6630 = CARTESIAN_POINT ( 'NONE',  ( -10.00000000000000000, 42.00000000000000000, 10.00000000000000000 ) ) ;
#6631 = ORIENTED_EDGE ( 'NONE', *, *, #4568, .T. ) ;
#6632 = AXIS2_PLACEMENT_3D ( 'NONE', #802, #5731, #326 ) ;
#6633 = ORIENTED_EDGE ( 'NONE', *, *, #3129, .T. ) ;
#6634 = LINE ( 'NONE', #10, #5800 ) ;
#6635 = CIRCLE ( 'NONE', #833, 199.9963296805737230 ) ;
#6636 = EDGE_CURVE ( 'NONE', #1540, #5426, #6588, .T. ) ;
#6637 = DIRECTION ( 'NONE',  ( 1.000000000000000000, 0.000000000000000000, 0.000000000000000000 ) ) ;
#6638 = DIRECTION ( 'NONE',  ( 0.000000000000000000, 0.000000000000000000, 1.000000000000000000 ) ) ;
#6639 = EDGE_CURVE ( 'NONE', #578, #2201, #5375, .T. ) ;
#6640 = ORIENTED_EDGE ( 'NONE', *, *, #3269, .F. ) ;
#6641 = EDGE_CURVE ( 'NONE', #738, #6698, #6956, .T. ) ;
#6642 = AXIS2_PLACEMENT_3D ( 'NONE', #7144, #1145, #2346 ) ;
#6643 = EDGE_CURVE ( 'NONE', #4328, #1219, #1304, .T. ) ;
#6644 = VERTEX_POINT ( 'NONE', #1756 ) ;
#6645 = CARTESIAN_POINT ( 'NONE',  ( -20.63749999999999929, 0.000000000000000000, -30.00000000000000000 ) ) ;
#6646 = CARTESIAN_POINT ( 'NONE',  ( 2.503857664561936813E-16, -9.237604307034025908, -4.700000000000000178 ) ) ;
#6647 = CARTESIAN_POINT ( 'NONE',  ( 0.000000000000000000, 0.000000000000000000, 10.00000000000000000 ) ) ;
#6648 = FACE_OUTER_BOUND ( 'NONE', #5651, .T. ) ;
#6649 = EDGE_CURVE ( 'NONE', #1582, #1609, #6458, .T. ) ;
#6650 = PLANE ( 'NONE',  #814 ) ;
#6651 = VERTEX_POINT ( 'NONE', #4187 ) ;
#6652 = AXIS2_PLACEMENT_3D ( 'NONE', #3447, #6486, #4075 ) ;
#6653 = DIRECTION ( 'NONE',  ( -0.000000000000000000, -0.000000000000000000, -1.000000000000000000 ) ) ;
#6654 = DIRECTION ( 'NONE',  ( -0.000000000000000000, 0.000000000000000000, 1.000000000000000000 ) ) ;
#6655 = DIRECTION ( 'NONE',  ( -0.000000000000000000, -0.000000000000000000, 1.000000000000000000 ) ) ;
#6656 = DIRECTION ( 'NONE',  ( 0.000000000000000000, 0.000000000000000000, 1.000000000000000000 ) ) ;
#6657 = DIRECTION ( 'NONE',  ( 1.000000000000000000, 0.000000000000000000, 0.000000000000000000 ) ) ;
#6658 = FACE_BOUND ( 'NONE', #2451, .T. ) ;
#6659 = UNCERTAINTY_MEASURE_WITH_UNIT (LENGTH_MEASURE( 1.000000000000000082E-05 ), #6276, 'distance_accuracy_value', 'NONE');
#6660 = DIRECTION ( 'NONE',  ( 0.000000000000000000, -1.000000000000000000, 0.000000000000000000 ) ) ;
#6661 = EDGE_LOOP ( 'NONE', ( #5847, #6858, #6088, #2878 ) ) ;
#6662 = ORIENTED_EDGE ( 'NONE', *, *, #2037, .T. ) ;
#6663 = AXIS2_PLACEMENT_3D ( 'NONE', #1885, #5396, #2994 ) ;
#6664 = VERTEX_POINT ( 'NONE', #4263 ) ;
#6665 = CARTESIAN_POINT ( 'NONE',  ( 85.00000000000000000, 9.720002580593245511E-13, 0.000000000000000000 ) ) ;
#6666 = FILL_AREA_STYLE_COLOUR ( '', #6747 ) ;
#6667 = CYLINDRICAL_SURFACE ( 'NONE', #4576, 35.97500000000000853 ) ;
#6668 = CIRCLE ( 'NONE', #6801, 37.49999999999997868 ) ;
#6669 = ORIENTED_EDGE ( 'NONE', *, *, #2077, .T. ) ;
#6670 = ORIENTED_EDGE ( 'NONE', *, *, #6979, .F. ) ;
#6671 = CIRCLE ( 'NONE', #3779, 5.249999999999991118 ) ;
#6672 = DIRECTION ( 'NONE',  ( 0.000000000000000000, 0.000000000000000000, 1.000000000000000000 ) ) ;
#6673 = CARTESIAN_POINT ( 'NONE',  ( -20.63749999999999929, 3.949485927250214050E-15, 32.25000000000000000 ) ) ;
#6674 = LINE ( 'NONE', #7306, #2184 ) ;
#6675 = ORIENTED_EDGE ( 'NONE', *, *, #327, .F. ) ;
#6676 = VECTOR ( 'NONE', #3932, 1000.000000000000000 ) ;
#6677 = ORIENTED_EDGE ( 'NONE', *, *, #2461, .T. ) ;
#6678 = PRODUCT_DEFINITION_SHAPE ( 'NONE', 'NONE',  #7772 ) ;
#6679 = LINE ( 'NONE', #1309, #4869 ) ;
#6680 = DIRECTION ( 'NONE',  ( 1.000000000000000000, 0.000000000000000000, 0.000000000000000000 ) ) ;
#6681 = AXIS2_PLACEMENT_3D ( 'NONE', #7653, #4143, #2267 ) ;
#6682 = FACE_BOUND ( 'NONE', #5578, .T. ) ;
#6683 = DIRECTION ( 'NONE',  ( 1.000000000000000000, 0.000000000000000000, 0.000000000000000000 ) ) ;
#6684 = UNCERTAINTY_MEASURE_WITH_UNIT (LENGTH_MEASURE( 1.000000000000000082E-05 ), #2818, 'distance_accuracy_value', 'NONE');
#6685 = ADVANCED_FACE ( 'NONE', ( #4226 ), #1189, .F. ) ;
#6686 = DIRECTION ( 'NONE',  ( -0.000000000000000000, -0.000000000000000000, 1.000000000000000000 ) ) ;
#6687 = EDGE_LOOP ( 'NONE', ( #4335, #4537, #2958, #1122 ) ) ;
#6688 = CIRCLE ( 'NONE', #7563, 5.000000000000004441 ) ;
#6689 = CARTESIAN_POINT ( 'NONE',  ( 279.9963296805736945, -6.783120157456498832E-12, 0.000000000000000000 ) ) ;
#6690 = ADVANCED_FACE ( 'NONE', ( #5333 ), #3601, .T. ) ;
#6691 = CARTESIAN_POINT ( 'NONE',  ( 3.199999999999994404, 0.000000000000000000, 0.000000000000000000 ) ) ;
#6692 = CARTESIAN_POINT ( 'NONE',  ( -10.00000000000000000, 41.99999999999999289, -60.00000000000000711 ) ) ;
#6693 = DIRECTION ( 'NONE',  ( 0.1045284632676645176, -0.9945218953682721796, 0.000000000000000000 ) ) ;
#6694 = CIRCLE ( 'NONE', #3291, 1.250000000000000444 ) ;
#6695 =( LENGTH_UNIT ( ) NAMED_UNIT ( * ) SI_UNIT ( .MILLI., .METRE. ) );
#6696 = CARTESIAN_POINT ( 'NONE',  ( 0.000000000000000000, 0.000000000000000000, -82.99999999999998579 ) ) ;
#6697 = DIRECTION ( 'NONE',  ( 1.000000000000000000, 0.000000000000000000, 0.000000000000000000 ) ) ;
#6698 = VERTEX_POINT ( 'NONE', #3639 ) ;
#6699 = ORIENTED_EDGE ( 'NONE', *, *, #5538, .T. ) ;
#6700 = PRODUCT_DEFINITION_CONTEXT ( 'detailed design', #6621, 'design' ) ;
#6701 = ORIENTED_EDGE ( 'NONE', *, *, #2592, .T. ) ;
#6702 = CARTESIAN_POINT ( 'NONE',  ( -28.49999999999999645, 3.490243377569956456E-15, 0.000000000000000000 ) ) ;
#6703 = CARTESIAN_POINT ( 'NONE',  ( 5.354491962338131295, -6.146186931204413284, -4.631901280394567166 ) ) ;
#6704 = CARTESIAN_POINT ( 'NONE',  ( 10.00000000000000000, 0.000000000000000000, 0.000000000000000000 ) ) ;
#6705 = ADVANCED_FACE ( 'NONE', ( #2933 ), #6047, .T. ) ;
#6706 = EDGE_LOOP ( 'NONE', ( #5839, #432, #3426, #5879 ) ) ;
#6707 = ORIENTED_EDGE ( 'NONE', *, *, #6211, .F. ) ;
#6708 = DIRECTION ( 'NONE',  ( 1.000000000000000000, 0.000000000000000000, 0.000000000000000000 ) ) ;
#6709 = DIRECTION ( 'NONE',  ( 1.000000000000000000, 1.776356839400250465E-15, 0.000000000000000000 ) ) ;
#6710 = DIRECTION ( 'NONE',  ( 1.000000000000000000, 0.000000000000000000, 0.000000000000000000 ) ) ;
#6711 = CIRCLE ( 'NONE', #1541, 150.0000000000000568 ) ;
#6712 = VERTEX_POINT ( 'NONE', #5489 ) ;
#6713 = AXIS2_PLACEMENT_3D ( 'NONE', #4760, #2871, #7167 ) ;
#6714 = ORIENTED_EDGE ( 'NONE', *, *, #2209, .T. ) ;
#6715 =( REPRESENTATION_RELATIONSHIP ('NONE','NONE', #1229, #2051 ) REPRESENTATION_RELATIONSHIP_WITH_TRANSFORMATION ( #2198 )SHAPE_REPRESENTATION_RELATIONSHIP( ) );
#6716 = FACE_OUTER_BOUND ( 'NONE', #4150, .T. ) ;
#6717 = DIRECTION ( 'NONE',  ( 5.551115123125782702E-17, -0.000000000000000000, 1.000000000000000000 ) ) ;
#6718 = VECTOR ( 'NONE', #6433, 1000.000000000000000 ) ;
#6719 = CARTESIAN_POINT ( 'NONE',  ( 4.586480920263560357, -37.21846574978686562, 0.000000000000000000 ) ) ;
#6720 = CARTESIAN_POINT ( 'NONE',  ( -32.49999999999997158, 0.000000000000000000, -93.00430309513780003 ) ) ;
#6721 = DIRECTION ( 'NONE',  ( 0.000000000000000000, 0.000000000000000000, -1.000000000000000000 ) ) ;
#6722 = PRODUCT_DEFINITION ( 'UNKNOWN', '', #3064, #2364 ) ;
#6723 = ORIENTED_EDGE ( 'NONE', *, *, #2501, .T. ) ;
#6724 = AXIS2_PLACEMENT_3D ( 'NONE', #5757, #1538, #5679 ) ;
#6725 = DIRECTION ( 'NONE',  ( -1.000000000000000000, 0.000000000000000000, -0.000000000000000000 ) ) ;
#6726 = DIRECTION ( 'NONE',  ( 1.000000000000000000, 0.000000000000000000, 0.000000000000000000 ) ) ;
#6727 = DIRECTION ( 'NONE',  ( 1.000000000000000000, 0.000000000000000000, -0.000000000000000000 ) ) ;
#6728 = CARTESIAN_POINT ( 'NONE',  ( -165.3429183184014732, 46.38600551860932342, 0.000000000000000000 ) ) ;
#6729 = COLOUR_RGB ( '',0.8941176470588234615, 0.8941176470588234615, 0.8941176470588234615 ) ;
#6730 = AXIS2_PLACEMENT_3D ( 'NONE', #5648, #240, #7534 ) ;
#6731 = CARTESIAN_POINT ( 'NONE',  ( 0.000000000000000000, 4.133182947122317561E-15, -33.75000000000000000 ) ) ;
#6732 = ADVANCED_FACE ( 'NONE', ( #6560 ), #1866, .F. ) ;
#6733 = DIRECTION ( 'NONE',  ( 1.000000000000000000, 0.000000000000000000, 0.000000000000000000 ) ) ;
#6734 = DIRECTION ( 'NONE',  ( -3.081487911019577365E-33, 2.775557561562891967E-17, 1.000000000000000000 ) ) ;
#6735 = EDGE_CURVE ( 'NONE', #4364, #587, #2504, .T. ) ;
#6736 = VERTEX_POINT ( 'NONE', #559 ) ;
#6737 = ADVANCED_FACE ( 'NONE', ( #5526 ), #5682, .T. ) ;
#6738 = EDGE_LOOP ( 'NONE', ( #6108, #7341, #7553, #6933 ) ) ;
#6739 =( GEOMETRIC_REPRESENTATION_CONTEXT ( 3 ) GLOBAL_UNCERTAINTY_ASSIGNED_CONTEXT ( ( #2514 ) ) GLOBAL_UNIT_ASSIGNED_CONTEXT ( ( #4283, #1284, #1209 ) ) REPRESENTATION_CONTEXT ( 'NONE', 'WORKASPACE' ) );
#6740 = EDGE_CURVE ( 'NONE', #6375, #1789, #5942, .T. ) ;
#6741 = VERTEX_POINT ( 'NONE', #3797 ) ;
#6742 = FACE_OUTER_BOUND ( 'NONE', #1365, .T. ) ;
#6743 = DIRECTION ( 'NONE',  ( 0.000000000000000000, 0.000000000000000000, -1.000000000000000000 ) ) ;
#6744 =( NAMED_UNIT ( * ) SI_UNIT ( $, .STERADIAN. ) SOLID_ANGLE_UNIT ( ) );
#6745 = CARTESIAN_POINT ( 'NONE',  ( 5.000000000000000888, 0.000000000000000000, -4.699999999999999289 ) ) ;
#6746 = EDGE_CURVE ( 'NONE', #6086, #924, #3559, .T. ) ;
#6747 = COLOUR_RGB ( '',1.000000000000000000, 0.9490196078431372140, 0.9098039215686274384 ) ;
#6748 = CLOSED_SHELL ( 'NONE', ( #6546, #2458, #7417, #4600, #4803, #358, #4754, #4708, #5541, #2780, #5671, #7532, #3935, #1038, #7651, #2694, #1137, #5041, #6976, #5203, #460, #1385, #4076, #220, #5177, #1617, #7321, #3950, #6732, #4218, #3604, #1192, #3807 ) ) ;
#6749 = ORIENTED_EDGE ( 'NONE', *, *, #2975, .T. ) ;
#6750 = PRODUCT ( 'stud long', 'stud long', '', ( #6219 ) ) ;
#6751 = EDGE_LOOP ( 'NONE', ( #2378, #4172, #3742, #6263, #3968, #2022, #5513, #2021 ) ) ;
#6752 = VERTEX_POINT ( 'NONE', #3760 ) ;
#6753 = EDGE_CURVE ( 'NONE', #3231, #1907, #7578, .T. ) ;
#6754 = UNCERTAINTY_MEASURE_WITH_UNIT (LENGTH_MEASURE( 1.000000000000000082E-05 ), #7406, 'distance_accuracy_value', 'NONE');
#6755 = VECTOR ( 'NONE', #3496, 1000.000000000000000 ) ;
#6756 = DIRECTION ( 'NONE',  ( -0.000000000000000000, -0.000000000000000000, 1.000000000000000000 ) ) ;
#6757 = DIRECTION ( 'NONE',  ( -0.000000000000000000, -0.000000000000000000, -1.000000000000000000 ) ) ;
#6758 = VECTOR ( 'NONE', #6653, 1000.000000000000000 ) ;
#6759 = CARTESIAN_POINT ( 'NONE',  ( 29.99999999999999289, 0.000000000000000000, -82.99999999999995737 ) ) ;
#6760 = ORIENTED_EDGE ( 'NONE', *, *, #2412, .T. ) ;
#6761 = ORIENTED_EDGE ( 'NONE', *, *, #4327, .T. ) ;
#6762 = CIRCLE ( 'NONE', #1984, 32.81578194438969120 ) ;
#6763 = DIRECTION ( 'NONE',  ( -0.000000000000000000, -0.000000000000000000, -1.000000000000000000 ) ) ;
#6764 = CARTESIAN_POINT ( 'NONE',  ( -0.3344772040064616925, 0.000000000000000000, 0.000000000000000000 ) ) ;
#6765 = FACE_OUTER_BOUND ( 'NONE', #4683, .T. ) ;
#6766 = DIRECTION ( 'NONE',  ( 0.000000000000000000, 0.000000000000000000, 1.000000000000000000 ) ) ;
#6767 = CARTESIAN_POINT ( 'NONE',  ( 4.250000000000000000, 0.000000000000000000, -4.700000000000000178 ) ) ;
#6768 = ORIENTED_EDGE ( 'NONE', *, *, #4084, .F. ) ;
#6769 = CIRCLE ( 'NONE', #6387, 29.99999999999999289 ) ;
#6770 = APPLICATION_CONTEXT ( 'automotive_design' ) ;
#6771 = DIRECTION ( 'NONE',  ( -0.000000000000000000, -0.000000000000000000, 1.000000000000000000 ) ) ;
#6772 = DIRECTION ( 'NONE',  ( 0.4999999999999979461, 0.8660254037844398178, 0.000000000000000000 ) ) ;
#6773 = VECTOR ( 'NONE', #2706, 1000.000000000000000 ) ;
#6774 = DIRECTION ( 'NONE',  ( -1.000000000000000000, 0.000000000000000000, 0.000000000000000000 ) ) ;
#6775 = CARTESIAN_POINT ( 'NONE',  ( -4.432034252711344102, 28.15327818181735964, -79.99999999999995737 ) ) ;
#6776 =( LENGTH_UNIT ( ) NAMED_UNIT ( * ) SI_UNIT ( .MILLI., .METRE. ) );
#6777 = FILL_AREA_STYLE ('',( #3150 ) ) ;
#6778 = PLANE ( 'NONE',  #1123 ) ;
#6779 = EDGE_LOOP ( 'NONE', ( #4766, #5368 ) ) ;
#6780 = VECTOR ( 'NONE', #3612, 1000.000000000000000 ) ;
#6781 = ORIENTED_EDGE ( 'NONE', *, *, #316, .T. ) ;
#6782 = EDGE_CURVE ( 'NONE', #1974, #147, #7420, .T. ) ;
#6783 = VERTEX_POINT ( 'NONE', #6166 ) ;
#6784 = FACE_OUTER_BOUND ( 'NONE', #553, .T. ) ;
#6785 = CARTESIAN_POINT ( 'NONE',  ( 89.90381056766497636, 75.00000000000153477, 10.00000000000000000 ) ) ;
#6786 = SURFACE_STYLE_USAGE ( .BOTH. , #2016 ) ;
#6787 = ADVANCED_FACE ( 'NONE', ( #2544 ), #3205, .F. ) ;
#6788 = AXIS2_PLACEMENT_3D ( 'NONE', #1664, #4062, #7732 ) ;
#6789 = CARTESIAN_POINT ( 'NONE',  ( 3.499999999999996003, 0.000000000000000000, -37.19999999999999574 ) ) ;
#6790 = ADVANCED_FACE ( 'NONE', ( #751 ), #4421, .F. ) ;
#6791 = ORIENTED_EDGE ( 'NONE', *, *, #6459, .T. ) ;
#6792 = ORIENTED_EDGE ( 'NONE', *, *, #5528, .T. ) ;
#6793 = AXIS2_PLACEMENT_3D ( 'NONE', #4831, #7206, #100 ) ;
#6794 = VERTEX_POINT ( 'NONE', #5643 ) ;
#6795 = VECTOR ( 'NONE', #2579, 1000.000000000000000 ) ;
#6796 = EDGE_CURVE ( 'NONE', #3517, #3380, #4188, .T. ) ;
#6797 = AXIS2_PLACEMENT_3D ( 'NONE', #4514, #7432, #2596 ) ;
#6798 = CARTESIAN_POINT ( 'NONE',  ( 207.8429183184020985, 119.9981648402868331, 10.00000000000000000 ) ) ;
#6799 = CARTESIAN_POINT ( 'NONE',  ( -20.63749999999999929, 0.000000000000000000, -32.25000000000000000 ) ) ;
#6800 = ORIENTED_EDGE ( 'NONE', *, *, #5086, .F. ) ;
#6801 = AXIS2_PLACEMENT_3D ( 'NONE', #2226, #2725, #4938 ) ;
#6802 = DIRECTION ( 'NONE',  ( -1.000000000000000000, 0.000000000000000000, 0.000000000000000000 ) ) ;
#6803 = PLANE ( 'NONE',  #1813 ) ;
#6804 = LINE ( 'NONE', #3288, #7400 ) ;
#6805 = AXIS2_PLACEMENT_3D ( 'NONE', #6221, #810, #1323 ) ;
#6806 = DIRECTION ( 'NONE',  ( 0.000000000000000000, 0.000000000000000000, 1.000000000000000000 ) ) ;
#6807 = VERTEX_POINT ( 'NONE', #6832 ) ;
#6808 = DIRECTION ( 'NONE',  ( -0.000000000000000000, -0.000000000000000000, 1.000000000000000000 ) ) ;
#6809 = AXIS2_PLACEMENT_3D ( 'NONE', #6343, #3899, #3420 ) ;
#6810 = DIRECTION ( 'NONE',  ( 1.000000000000000000, 0.000000000000000000, 0.000000000000000000 ) ) ;
#6811 = FACE_OUTER_BOUND ( 'NONE', #4413, .T. ) ;
#6812 = FACE_OUTER_BOUND ( 'NONE', #3967, .T. ) ;
#6813 = DIRECTION ( 'NONE',  ( -0.9987395008963458887, -0.05019371822567170183, -2.550145071705742900E-17 ) ) ;
#6814 = PRODUCT_DEFINITION_SHAPE ( 'NONE', 'NONE',  #7780 ) ;
#6815 =( NAMED_UNIT ( * ) SI_UNIT ( $, .STERADIAN. ) SOLID_ANGLE_UNIT ( ) );
#6816 = DIRECTION ( 'NONE',  ( 1.000000000000000000, 0.000000000000000000, 0.000000000000000000 ) ) ;
#6817 = AXIS2_PLACEMENT_3D ( 'NONE', #4224, #6672, #1300 ) ;
#6818 = ORIENTED_EDGE ( 'NONE', *, *, #6639, .F. ) ;
#6819 = VERTEX_POINT ( 'NONE', #6759 ) ;
#6820 = ORIENTED_EDGE ( 'NONE', *, *, #2628, .T. ) ;
#6821 = ORIENTED_EDGE ( 'NONE', *, *, #7219, .T. ) ;
#6822 = AXIS2_PLACEMENT_3D ( 'NONE', #6038, #3077, #1894 ) ;
#6823 = CYLINDRICAL_SURFACE ( 'NONE', #6069, 5.250000000000000888 ) ;
#6824 = CARTESIAN_POINT ( 'NONE',  ( -4.494751301858288528, -36.47409643479112162, -3.000000000000000000 ) ) ;
#6825 = DIRECTION ( 'NONE',  ( 1.000000000000000000, 0.000000000000000000, 0.000000000000000000 ) ) ;
#6826 = VERTEX_POINT ( 'NONE', #2107 ) ;
#6827 =( REPRESENTATION_RELATIONSHIP ('NONE','NONE', #1229, #2051 ) REPRESENTATION_RELATIONSHIP_WITH_TRANSFORMATION ( #5816 )SHAPE_REPRESENTATION_RELATIONSHIP( ) );
#6828 = ORIENTED_EDGE ( 'NONE', *, *, #2752, .T. ) ;
#6829 = EDGE_CURVE ( 'NONE', #2329, #980, #2741, .T. ) ;
#6830 = CARTESIAN_POINT ( 'NONE',  ( 129.9038105676665396, -74.99999999999882050, 0.000000000000000000 ) ) ;
#6831 = DIRECTION ( 'NONE',  ( 0.9808248999643442989, 0.1948910352220800113, -5.550004789056643899E-17 ) ) ;
#6832 = CARTESIAN_POINT ( 'NONE',  ( -9.999999999999998224, 28.28427124746189847, 10.00000000000000000 ) ) ;
#6833 = VERTEX_POINT ( 'NONE', #1382 ) ;
#6834 = EDGE_CURVE ( 'NONE', #6615, #7307, #7218, .T. ) ;
#6835 = CIRCLE ( 'NONE', #7575, 1.250000000000000444 ) ;
#6836 = ADVANCED_FACE ( 'NONE', ( #3718 ), #2654, .F. ) ;
#6837 = DIRECTION ( 'NONE',  ( 0.000000000000000000, 0.000000000000000000, 1.000000000000000000 ) ) ;
#6838 = CYLINDRICAL_SURFACE ( 'NONE', #423, 5.249999999999983125 ) ;
#6839 = CARTESIAN_POINT ( 'NONE',  ( 0.000000000000000000, 0.000000000000000000, 10.00000000000000888 ) ) ;
#6840 = AXIS2_PLACEMENT_3D ( 'NONE', #6869, #271, #5564 ) ;
#6841 = PRODUCT_DEFINITION_FORMATION_WITH_SPECIFIED_SOURCE ( 'ANY', '', #2099, .NOT_KNOWN. ) ;
#6842 = DIRECTION ( 'NONE',  ( -0.000000000000000000, -0.000000000000000000, 1.000000000000000000 ) ) ;
#6843 = VERTEX_POINT ( 'NONE', #6125 ) ;
#6844 = EDGE_CURVE ( 'NONE', #6002, #886, #5050, .T. ) ;
#6845 = CARTESIAN_POINT ( 'NONE',  ( 5.777789833161707559E-31, -4.119912841284263785E-15, -119.9999999999999716 ) ) ;
#6846 = CIRCLE ( 'NONE', #2826, 37.49999999999997868 ) ;
#6847 = DIRECTION ( 'NONE',  ( 0.000000000000000000, 0.000000000000000000, -1.000000000000000000 ) ) ;
#6848 = EDGE_CURVE ( 'NONE', #7232, #3132, #3432, .T. ) ;
#6849 = DIRECTION ( 'NONE',  ( 1.000000000000000000, 0.000000000000000000, 0.000000000000000000 ) ) ;
#6850 = CYLINDRICAL_SURFACE ( 'NONE', #3749, 1.250000000000000222 ) ;
#6851 = DIRECTION ( 'NONE',  ( -1.075821697160534305E-16, -3.917227599481534893E-17, 0.9999999999999998890 ) ) ;
#6852 = CARTESIAN_POINT ( 'NONE',  ( 4.494751301858288528, -36.47409643479112162, -3.000000000000000000 ) ) ;
#6853 = CARTESIAN_POINT ( 'NONE',  ( 0.000000000000000000, 0.000000000000000000, -82.99999999999998579 ) ) ;
#6854 = VECTOR ( 'NONE', #1787, 1000.000000000000000 ) ;
#6855 = EDGE_LOOP ( 'NONE', ( #1600, #3640, #2722, #2815 ) ) ;
#6856 = ORIENTED_EDGE ( 'NONE', *, *, #4071, .T. ) ;
#6857 = ORIENTED_EDGE ( 'NONE', *, *, #2685, .T. ) ;
#6858 = ORIENTED_EDGE ( 'NONE', *, *, #6359, .F. ) ;
#6859 = FACE_BOUND ( 'NONE', #1708, .T. ) ;
#6860 = DIRECTION ( 'NONE',  ( 0.000000000000000000, 0.000000000000000000, 1.000000000000000000 ) ) ;
#6861 =( LENGTH_UNIT ( ) NAMED_UNIT ( * ) SI_UNIT ( .MILLI., .METRE. ) );
#6862 = CYLINDRICAL_SURFACE ( 'NONE', #5842, 4.999999999999990230 ) ;
#6863 = ORIENTED_EDGE ( 'NONE', *, *, #662, .F. ) ;
#6864 = VERTEX_POINT ( 'NONE', #2303 ) ;
#6865 = CARTESIAN_POINT ( 'NONE',  ( -7.039801714450301422E-15, 0.000000000000000000, -82.99999999999995737 ) ) ;
#6866 = CONICAL_SURFACE ( 'NONE', #4217, 8.000000000000000000, 1.047197551196596299 ) ;
#6867 = STYLED_ITEM ( 'NONE', ( #2289 ), #1052 ) ;
#6868 = DIRECTION ( 'NONE',  ( 0.9845265360683707057, 0.1752355551171480841, 0.000000000000000000 ) ) ;
#6869 = CARTESIAN_POINT ( 'NONE',  ( -129.9038105676655164, -75.00000000000063949, 10.00000000000000000 ) ) ;
#6870 = VERTEX_POINT ( 'NONE', #6394 ) ;
#6871 = AXIS2_PLACEMENT_3D ( 'NONE', #1811, #1246, #1542 ) ;
#6872 = PRODUCT_DEFINITION_SHAPE ( 'NONE', 'NONE',  #7766 ) ;
#6873 = EDGE_CURVE ( 'NONE', #7260, #7478, #6356, .T. ) ;
#6874 = DIRECTION ( 'NONE',  ( 3.081487911019577365E-33, -2.775557561562891967E-17, -1.000000000000000000 ) ) ;
#6875 = DIRECTION ( 'NONE',  ( 1.000000000000000000, 0.000000000000000000, 0.000000000000000000 ) ) ;
#6876 = AXIS2_PLACEMENT_3D ( 'NONE', #876, #6847, #247 ) ;
#6877 = LINE ( 'NONE', #1391, #4119 ) ;
#6878 = EDGE_CURVE ( 'NONE', #2235, #5165, #4566, .T. ) ;
#6879 = EDGE_CURVE ( 'NONE', #4484, #3551, #6085, .T. ) ;
#6880 = DIRECTION ( 'NONE',  ( 0.000000000000000000, 0.000000000000000000, 1.000000000000000000 ) ) ;
#6881 = EDGE_LOOP ( 'NONE', ( #7500, #3629, #7530, #7142, #5537, #3103, #3925, #3789, #3941, #4654, #165, #4868 ) ) ;
#6882 = ADVANCED_FACE ( 'NONE', ( #7022 ), #6946, .F. ) ;
#6883 = VECTOR ( 'NONE', #3293, 1000.000000000000000 ) ;
#6884 = DIRECTION ( 'NONE',  ( -5.551115123125782702E-17, 0.000000000000000000, -1.000000000000000000 ) ) ;
#6885 = DIRECTION ( 'NONE',  ( -0.000000000000000000, -0.000000000000000000, -1.000000000000000000 ) ) ;
#6886 = FACE_OUTER_BOUND ( 'NONE', #3778, .T. ) ;
#6887 = EDGE_CURVE ( 'NONE', #421, #5007, #5249, .T. ) ;
#6888 = DIRECTION ( 'NONE',  ( -1.000000000000000000, 0.000000000000000000, -0.000000000000000000 ) ) ;
#6889 = PRODUCT_CONTEXT ( 'NONE', #7419, 'mechanical' ) ;
#6890 = EDGE_CURVE ( 'NONE', #3121, #4116, #1243, .T. ) ;
#6891 = AXIS2_PLACEMENT_3D ( 'NONE', #4539, #1543, #5210 ) ;
#6892 =( NAMED_UNIT ( * ) PLANE_ANGLE_UNIT ( ) SI_UNIT ( $, .RADIAN. ) );
#6893 = EDGE_LOOP ( 'NONE', ( #1041, #6931, #5738, #6242, #3534, #232, #2649, #5071, #3352, #2313, #7639, #1991, #4170, #832, #7280 ) ) ;
#6894 = ORIENTED_EDGE ( 'NONE', *, *, #3073, .T. ) ;
#6895 = ORIENTED_EDGE ( 'NONE', *, *, #7688, .T. ) ;
#6896 = AXIS2_PLACEMENT_3D ( 'NONE', #6845, #3253, #4432 ) ;
#6897 = VERTEX_POINT ( 'NONE', #349 ) ;
#6898 = B_SPLINE_CURVE_WITH_KNOTS ( 'NONE', 3,
 ( #1168, #2336, #1090, #1128, #585, #1777 ),
 .UNSPECIFIED., .F., .F.,
 ( 4, 2, 4 ),
 ( 2.380731629581968059E-07, 0.002336973833157553800, 0.004673709593152148775 ),
 .UNSPECIFIED. ) ;
#6899 = PLANE ( 'NONE',  #258 ) ;
#6900 = DIRECTION ( 'NONE',  ( 0.000000000000000000, 0.000000000000000000, -1.000000000000000000 ) ) ;
#6901 = CARTESIAN_POINT ( 'NONE',  ( -68.76644452187068168, 49.96174644486002592, 0.000000000000000000 ) ) ;
#6902 = AXIS2_PLACEMENT_3D ( 'NONE', #1245, #6655, #3148 ) ;
#6903 = VERTEX_POINT ( 'NONE', #5206 ) ;
#6904 = VERTEX_POINT ( 'NONE', #903 ) ;
#6905 = ORIENTED_EDGE ( 'NONE', *, *, #4608, .T. ) ;
#6906 = AXIS2_PLACEMENT_3D ( 'NONE', #1077, #4036, #5344 ) ;
#6907 = CARTESIAN_POINT ( 'NONE',  ( 0.000000000000000000, 0.000000000000000000, -4.700000000000000178 ) ) ;
#6908 = DIRECTION ( 'NONE',  ( -0.000000000000000000, -0.000000000000000000, 1.000000000000000000 ) ) ;
#6909 = CARTESIAN_POINT ( 'NONE',  ( 0.6527133886630217541, -8.860760056385757366, -0.4969600502617634863 ) ) ;
#6910 = ORIENTED_EDGE ( 'NONE', *, *, #4964, .F. ) ;
#6911 = B_SPLINE_CURVE_WITH_KNOTS ( 'NONE', 3,
 ( #3744, #3078, #1367, #6703, #777, #4844 ),
 .UNSPECIFIED., .F., .F.,
 ( 4, 2, 4 ),
 ( 2.380731629582276432E-07, 0.002336973833157553367, 0.004673709593152147908 ),
 .UNSPECIFIED. ) ;
#6912 = CIRCLE ( 'NONE', #480, 28.50000000000000355 ) ;
#6913 = DIRECTION ( 'NONE',  ( 0.9412010056177179118, 0.3378471059875997051, 0.000000000000000000 ) ) ;
#6914 = CARTESIAN_POINT ( 'NONE',  ( 114.7481648402866483, 207.8429183184022122, -50.00000000000000000 ) ) ;
#6915 = APPLICATION_CONTEXT ( 'automotive_design' ) ;
#6916 = DIRECTION ( 'NONE',  ( -1.000000000000000000, 0.000000000000000000, 0.000000000000000000 ) ) ;
#6917 = DIRECTION ( 'NONE',  ( -0.000000000000000000, -0.000000000000000000, 1.000000000000000000 ) ) ;
#6918 = ORIENTED_EDGE ( 'NONE', *, *, #4620, .F. ) ;
#6919 = CIRCLE ( 'NONE', #3268, 29.99999999999999289 ) ;
#6920 = FACE_OUTER_BOUND ( 'NONE', #2377, .T. ) ;
#6921 = DIRECTION ( 'NONE',  ( 1.000000000000000000, 0.000000000000000000, 0.000000000000000000 ) ) ;
#6922 = VECTOR ( 'NONE', #4440, 1000.000000000000000 ) ;
#6923 = CARTESIAN_POINT ( 'NONE',  ( -5.000000000000000888, 0.000000000000000000, -4.674599999999997202 ) ) ;
#6924 = EDGE_CURVE ( 'NONE', #6223, #6189, #7090, .T. ) ;
#6925 = DIRECTION ( 'NONE',  ( 0.000000000000000000, 0.000000000000000000, 1.000000000000000000 ) ) ;
#6926 = DIRECTION ( 'NONE',  ( 0.000000000000000000, 0.000000000000000000, 1.000000000000000000 ) ) ;
#6927 = SURFACE_STYLE_FILL_AREA ( #7473 ) ;
#6928 = ORIENTED_EDGE ( 'NONE', *, *, #5812, .F. ) ;
#6929 = VERTEX_POINT ( 'NONE', #1659 ) ;
#6930 = AXIS2_PLACEMENT_3D ( 'NONE', #5704, #6900, #1528 ) ;
#6931 = ORIENTED_EDGE ( 'NONE', *, *, #354, .T. ) ;
#6932 = ADVANCED_FACE ( 'NONE', ( #4652 ), #1546, .T. ) ;
#6933 = ORIENTED_EDGE ( 'NONE', *, *, #6197, .T. ) ;
#6934 = CARTESIAN_POINT ( 'NONE',  ( 10.16320117273318679, -26.62629042736811869, -119.9999999999999716 ) ) ;
#6935 = DIRECTION ( 'NONE',  ( -1.000000000000000000, 0.000000000000000000, 0.000000000000000000 ) ) ;
#6936 = CIRCLE ( 'NONE', #4918, 5.249999999999976907 ) ;
#6937 = CARTESIAN_POINT ( 'NONE',  ( 0.000000000000000000, 0.000000000000000000, -50.00000000000000000 ) ) ;
#6938 = ORIENTED_EDGE ( 'NONE', *, *, #4042, .T. ) ;
#6939 = EDGE_CURVE ( 'NONE', #4674, #4251, #6338, .T. ) ;
#6940 = ORIENTED_EDGE ( 'NONE', *, *, #3073, .F. ) ;
#6941 = CIRCLE ( 'NONE', #2660, 35.25000000000000000 ) ;
#6942 = VERTEX_POINT ( 'NONE', #5719 ) ;
#6943 = DIRECTION ( 'NONE',  ( 5.551115123125782702E-17, 0.000000000000000000, 1.000000000000000000 ) ) ;
#6944 = EDGE_CURVE ( 'NONE', #5491, #5609, #2767, .T. ) ;
#6945 = CARTESIAN_POINT ( 'NONE',  ( -63.51644452187067458, 49.96174644486002592, 10.00000000000000000 ) ) ;
#6946 = CYLINDRICAL_SURFACE ( 'NONE', #3943, 5.249999999999976907 ) ;
#6947 = ORIENTED_EDGE ( 'NONE', *, *, #6305, .T. ) ;
#6948 = CYLINDRICAL_SURFACE ( 'NONE', #7007, 1.250000000000000444 ) ;
#6949 = FACE_OUTER_BOUND ( 'NONE', #2516, .T. ) ;
#6950 = LINE ( 'NONE', #3953, #3379 ) ;
#6951 = FACE_OUTER_BOUND ( 'NONE', #1289, .T. ) ;
#6952 = AXIS2_PLACEMENT_3D ( 'NONE', #3251, #4351, #3213 ) ;
#6953 = ORIENTED_EDGE ( 'NONE', *, *, #1871, .T. ) ;
#6954 = FACE_OUTER_BOUND ( 'NONE', #1034, .T. ) ;
#6955 = CARTESIAN_POINT ( 'NONE',  ( 5.857142857142855874, 0.000000000000000000, 9.480888224575629408 ) ) ;
#6956 = CIRCLE ( 'NONE', #782, 0.3000000000000016542 ) ;
#6957 = DIRECTION ( 'NONE',  ( -0.000000000000000000, -0.000000000000000000, 1.000000000000000000 ) ) ;
#6958 = AXIS2_PLACEMENT_3D ( 'NONE', #2631, #2598, #3733 ) ;
#6959 = EDGE_CURVE ( 'NONE', #1194, #5183, #6711, .T. ) ;
#6960 = PLANE ( 'NONE',  #3641 ) ;
#6961 = DIRECTION ( 'NONE',  ( 0.000000000000000000, 0.000000000000000000, 1.000000000000000000 ) ) ;
#6962 = ITEM_DEFINED_TRANSFORMATION ( 'NONE', 'NONE', #5230,  #7485 ) ;
#6963 = DIRECTION ( 'NONE',  ( 0.01999999999999999001, -0.9997999799959990108, 0.000000000000000000 ) ) ;
#6964 = ORIENTED_EDGE ( 'NONE', *, *, #3261, .T. ) ;
#6965 = ORIENTED_EDGE ( 'NONE', *, *, #4462, .T. ) ;
#6966 = CIRCLE ( 'NONE', #4063, 5.250000000000000888 ) ;
#6967 = ORIENTED_EDGE ( 'NONE', *, *, #2259, .T. ) ;
#6968 = CARTESIAN_POINT ( 'NONE',  ( -4.432034252711344102, 28.15327818181735964, -79.99999999999995737 ) ) ;
#6969 = DIRECTION ( 'NONE',  ( 0.000000000000000000, 0.000000000000000000, 1.000000000000000000 ) ) ;
#6970 = EDGE_CURVE ( 'NONE', #1194, #1572, #5284, .T. ) ;
#6971 = CARTESIAN_POINT ( 'NONE',  ( 8.000000000000000000, -3.867591403079175372, -0.4976753153245848660 ) ) ;
#6972 = CARTESIAN_POINT ( 'NONE',  ( -32.81578194438969120, 1.484218055610309728, -3.000000000000000000 ) ) ;
#6973 =( NAMED_UNIT ( * ) SI_UNIT ( $, .STERADIAN. ) SOLID_ANGLE_UNIT ( ) );
#6974 = CIRCLE ( 'NONE', #3575, 28.50000000000000355 ) ;
#6975 = DIRECTION ( 'NONE',  ( -0.9342558044690566499, -0.3566035499204627257, -1.650722232431654112E-17 ) ) ;
#6976 = ADVANCED_FACE ( 'NONE', ( #6321 ), #7569, .F. ) ;
#6977 = EDGE_CURVE ( 'NONE', #7680, #3299, #3319, .T. ) ;
#6978 = ORIENTED_EDGE ( 'NONE', *, *, #4315, .T. ) ;
#6979 = EDGE_CURVE ( 'NONE', #6736, #2383, #7609, .T. ) ;
#6980 = ORIENTED_EDGE ( 'NONE', *, *, #4507, .T. ) ;
#6981 = VECTOR ( 'NONE', #7579, 1000.000000000000000 ) ;
#6982 = VERTEX_POINT ( 'NONE', #3430 ) ;
#6983 = CYLINDRICAL_SURFACE ( 'NONE', #7690, 29.99999999999999289 ) ;
#6984 = EDGE_CURVE ( 'NONE', #7368, #6741, #5837, .T. ) ;
#6985 = CARTESIAN_POINT ( 'NONE',  ( 21.01644452187122170, -80.83980388508783221, 0.000000000000000000 ) ) ;
#6986 = CARTESIAN_POINT ( 'NONE',  ( 0.000000000000000000, 0.000000000000000000, 20.00000000000000000 ) ) ;
#6987 = ORIENTED_EDGE ( 'NONE', *, *, #5047, .T. ) ;
#6988 = AXIS2_PLACEMENT_3D ( 'NONE', #7436, #882, #2046 ) ;
#6989 = COLOUR_RGB ( '',0.8941176470588234615, 0.8941176470588234615, 0.8941176470588234615 ) ;
#6990 = DIRECTION ( 'NONE',  ( 0.000000000000000000, -1.000000000000000000, 0.000000000000000000 ) ) ;
#6991 = CARTESIAN_POINT ( 'NONE',  ( 1.469553684752138043E-14, 239.9963296805737230, 10.00000000000000000 ) ) ;
#6992 = CARTESIAN_POINT ( 'NONE',  ( -63.76644452187073142, 49.96174644486006855, -134.1720000000000255 ) ) ;
#6993 = DIRECTION ( 'NONE',  ( 0.1948910352220799280, -0.9808248999643441879, -1.110223024625155793E-18 ) ) ;
#6994 = ORIENTED_EDGE ( 'NONE', *, *, #997, .T. ) ;
#6995 = AXIS2_PLACEMENT_3D ( 'NONE', #4720, #7595, #1646 ) ;
#6996 = CARTESIAN_POINT ( 'NONE',  ( -8.000000000000000000, -4.618802153517013842, -0.7145311798163319628 ) ) ;
#6997 = FILL_AREA_STYLE_COLOUR ( '', #6376 ) ;
#6998 = CARTESIAN_POINT ( 'NONE',  ( 10.00000000000000000, 0.000000000000000000, -50.00000000000000000 ) ) ;
#6999 = CYLINDRICAL_SURFACE ( 'NONE', #1884, 5.250000000000004441 ) ;
#7000 = LINE ( 'NONE', #1596, #600 ) ;
#7001 = ITEM_DEFINED_TRANSFORMATION ( 'NONE', 'NONE', #6871,  #7485 ) ;
#7002 = DIRECTION ( 'NONE',  ( -1.000000000000000000, 0.000000000000000000, 0.000000000000000000 ) ) ;
#7003 = VERTEX_POINT ( 'NONE', #1852 ) ;
#7004 = ORIENTED_EDGE ( 'NONE', *, *, #6848, .F. ) ;
#7005 = ORIENTED_EDGE ( 'NONE', *, *, #470, .F. ) ;
#7006 = CARTESIAN_POINT ( 'NONE',  ( -5.354491962338124189, 6.146186931204407067, -4.631901280394571607 ) ) ;
#7007 = AXIS2_PLACEMENT_3D ( 'NONE', #4693, #984, #3477 ) ;
#7008 = CARTESIAN_POINT ( 'NONE',  ( 0.000000000000000000, 0.000000000000000000, 0.000000000000000000 ) ) ;
#7009 = DIRECTION ( 'NONE',  ( 1.000000000000000000, 0.000000000000000000, 0.000000000000000000 ) ) ;
#7010 = CARTESIAN_POINT ( 'NONE',  ( -6.873268260756527152E-15, 0.000000000000000000, -79.99999999999995737 ) ) ;
#7011 = DIRECTION ( 'NONE',  ( -0.000000000000000000, -0.000000000000000000, -1.000000000000000000 ) ) ;
#7012 = ORIENTED_EDGE ( 'NONE', *, *, #2415, .T. ) ;
#7013 = AXIS2_PLACEMENT_3D ( 'NONE', #7703, #6523, #4628 ) ;
#7014 = EDGE_CURVE ( 'NONE', #322, #3277, #68, .T. ) ;
#7015 = ORIENTED_EDGE ( 'NONE', *, *, #6164, .F. ) ;
#7016 = VERTEX_POINT ( 'NONE', #5435 ) ;
#7017 = ADVANCED_FACE ( 'NONE', ( #6512 ), #1169, .T. ) ;
#7018 = DIRECTION ( 'NONE',  ( 1.000000000000000000, 0.000000000000000000, 0.000000000000000000 ) ) ;
#7019 = CIRCLE ( 'NONE', #210, 0.7500000000000041078 ) ;
#7020 = EDGE_CURVE ( 'NONE', #1170, #1212, #3737, .T. ) ;
#7021 = DIRECTION ( 'NONE',  ( 1.000000000000000000, -1.224646799147352961E-16, 0.000000000000000000 ) ) ;
#7022 = FACE_OUTER_BOUND ( 'NONE', #4256, .T. ) ;
#7023 = ORIENTED_EDGE ( 'NONE', *, *, #1339, .F. ) ;
#7024 = ORIENTED_EDGE ( 'NONE', *, *, #3226, .T. ) ;
#7025 = VECTOR ( 'NONE', #761, 1000.000000000000000 ) ;
#7026 = ADVANCED_FACE ( 'NONE', ( #6145, #1100, #4837, #5548, #3037, #7251 ), #4247, .F. ) ;
#7027 = DIRECTION ( 'NONE',  ( 1.000000000000000000, 0.000000000000000000, 0.000000000000000000 ) ) ;
#7028 = CARTESIAN_POINT ( 'NONE',  ( 31.51644452187122525, -80.83980388508783221, 0.000000000000000000 ) ) ;
#7029 = DIRECTION ( 'NONE',  ( 0.3566035499204626702, -0.9342558044690565389, 2.649161120199466423E-17 ) ) ;
#7030 = VECTOR ( 'NONE', #4186, 1000.000000000000000 ) ;
#7031 = DIRECTION ( 'NONE',  ( -0.3189555096957539804, 0.9477696887085605981, -2.581026109104742702E-17 ) ) ;
#7032 = ORIENTED_EDGE ( 'NONE', *, *, #3309, .T. ) ;
#7033 = VERTEX_POINT ( 'NONE', #146 ) ;
#7034 = AXIS2_PLACEMENT_3D ( 'NONE', #1244, #6098, #4872 ) ;
#7035 = CARTESIAN_POINT ( 'NONE',  ( -63.51644452187023404, -49.96174644486060856, 10.00000000000000000 ) ) ;
#7036 = DIRECTION ( 'NONE',  ( 0.000000000000000000, 0.000000000000000000, 1.000000000000000000 ) ) ;
#7037 = FACE_OUTER_BOUND ( 'NONE', #5969, .T. ) ;
#7038 = DIRECTION ( 'NONE',  ( 1.000000000000000000, 0.000000000000000000, 0.000000000000000000 ) ) ;
#7039 = DIRECTION ( 'NONE',  ( 0.000000000000000000, 0.000000000000000000, 1.000000000000000000 ) ) ;
#7040 = EDGE_CURVE ( 'NONE', #6086, #294, #2577, .T. ) ;
#7041 = CONTEXT_DEPENDENT_SHAPE_REPRESENTATION ( #6715, #4478 ) ;
#7042 = DIRECTION ( 'NONE',  ( 1.000000000000000000, 0.000000000000000000, 0.000000000000000000 ) ) ;
#7043 = ORIENTED_EDGE ( 'NONE', *, *, #268, .F. ) ;
#7044 = VERTEX_POINT ( 'NONE', #1286 ) ;
#7045 = ORIENTED_EDGE ( 'NONE', *, *, #3978, .T. ) ;
#7046 = AXIS2_PLACEMENT_3D ( 'NONE', #1439, #6260, #847 ) ;
#7047 = DIRECTION ( 'NONE',  ( 1.000000000000000000, 0.000000000000000000, 0.000000000000000000 ) ) ;
#7048 = CARTESIAN_POINT ( 'NONE',  ( 4.000000000000004441, 6.928203230275507885, 0.000000000000000000 ) ) ;
#7049 = DIRECTION ( 'NONE',  ( 1.000000000000000000, 0.000000000000000000, 0.000000000000000000 ) ) ;
#7050 = DIRECTION ( 'NONE',  ( 1.000000000000000000, 0.000000000000000000, 0.000000000000000000 ) ) ;
#7051 = CARTESIAN_POINT ( 'NONE',  ( -213.0929183184020701, 119.9981648402869467, 10.00000000000000178 ) ) ;
#7052 = CARTESIAN_POINT ( 'NONE',  ( 3.199999999999994404, 0.000000000000000000, -37.50000000000000000 ) ) ;
#7053 = ORIENTED_EDGE ( 'NONE', *, *, #4512, .F. ) ;
#7054 = ORIENTED_EDGE ( 'NONE', *, *, #1830, .F. ) ;
#7055 = EDGE_LOOP ( 'NONE', ( #343, #4818, #6224, #2494 ) ) ;
#7056 = DIRECTION ( 'NONE',  ( 0.000000000000000000, 0.000000000000000000, 1.000000000000000000 ) ) ;
#7057 = CARTESIAN_POINT ( 'NONE',  ( 9.090232026328989079, -27.01143612819398143, -122.9999999999999716 ) ) ;
#7058 = DIRECTION ( 'NONE',  ( -0.000000000000000000, -0.000000000000000000, 1.000000000000000000 ) ) ;
#7059 = PRODUCT_DEFINITION ( 'UNKNOWN', '', #7221, #1456 ) ;
#7060 = DIRECTION ( 'NONE',  ( 0.000000000000000000, 0.000000000000000000, 1.000000000000000000 ) ) ;
#7061 = EDGE_LOOP ( 'NONE', ( #2935, #6118, #5560, #3564 ) ) ;
#7062 = AXIS2_PLACEMENT_3D ( 'NONE', #3587, #5996, #4214 ) ;
#7063 = CARTESIAN_POINT ( 'NONE',  ( -6.873268260756527152E-15, 0.000000000000000000, -79.99999999999995737 ) ) ;
#7064 = DIRECTION ( 'NONE',  ( 5.551115123125782702E-17, -0.000000000000000000, 1.000000000000000000 ) ) ;
#7065 = CIRCLE ( 'NONE', #5681, 28.49999999999999645 ) ;
#7066 = DIRECTION ( 'NONE',  ( 0.000000000000000000, 0.000000000000000000, 1.000000000000000000 ) ) ;
#7067 = CARTESIAN_POINT ( 'NONE',  ( 2.718977167127996530, 29.87653198021210699, -139.9999999999999716 ) ) ;
#7068 = EDGE_CURVE ( 'NONE', #6427, #1238, #2490, .T. ) ;
#7069 = EDGE_LOOP ( 'NONE', ( #4012, #3267 ) ) ;
#7070 = EDGE_LOOP ( 'NONE', ( #3663, #7093, #6195, #2937 ) ) ;
#7071 = EDGE_CURVE ( 'NONE', #1401, #5644, #1299, .T. ) ;
#7072 = CARTESIAN_POINT ( 'NONE',  ( -4.339467034331195627, -6.732211846623401108, -1.075167154381460273E-15 ) ) ;
#7073 = SURFACE_SIDE_STYLE ('',( #2900 ) ) ;
#7074 = DIRECTION ( 'NONE',  ( -0.000000000000000000, 1.000000000000000000, 1.224646799147353207E-16 ) ) ;
#7075 = DIRECTION ( 'NONE',  ( 0.5000000000000101030, -0.8660254037844328234, 0.000000000000000000 ) ) ;
#7076 = EDGE_CURVE ( 'NONE', #4919, #6651, #6966, .T. ) ;
#7077 = B_SPLINE_CURVE_WITH_KNOTS ( 'NONE', 3,
 ( #5891, #2320, #6567, #713, #7740, #2359 ),
 .UNSPECIFIED., .F., .F.,
 ( 4, 2, 4 ),
 ( 0.01291313371729457642, 0.01525081363757309350, 0.01758849355785160884 ),
 .UNSPECIFIED. ) ;
#7078 = DIRECTION ( 'NONE',  ( -1.000000000000000000, 0.000000000000000000, 0.000000000000000000 ) ) ;
#7079 = ORIENTED_EDGE ( 'NONE', *, *, #2358, .T. ) ;
#7080 = ORIENTED_EDGE ( 'NONE', *, *, #2928, .T. ) ;
#7081 = EDGE_LOOP ( 'NONE', ( #264, #5557, #2606, #1267 ) ) ;
#7082 = EDGE_CURVE ( 'NONE', #4200, #2474, #2565, .T. ) ;
#7083 = VECTOR ( 'NONE', #481, 1000.000000000000000 ) ;
#7084 = CARTESIAN_POINT ( 'NONE',  ( -202.5929183184026954, 119.9981648402859378, -120.0000000000000000 ) ) ;
#7085 = CARTESIAN_POINT ( 'NONE',  ( 10.69810649761388177, -28.02767413407170238, -139.9999999999999716 ) ) ;
#7086 = CYLINDRICAL_SURFACE ( 'NONE', #4749, 40.00000000000000711 ) ;
#7087 = DIRECTION ( 'NONE',  ( 1.000000000000000000, 0.000000000000000000, 0.000000000000000000 ) ) ;
#7088 = FACE_OUTER_BOUND ( 'NONE', #1482, .T. ) ;
#7089 = CYLINDRICAL_SURFACE ( 'NONE', #2019, 150.0000000000000568 ) ;
#7090 = CIRCLE ( 'NONE', #3687, 279.9963296805736945 ) ;
#7091 = ORIENTED_EDGE ( 'NONE', *, *, #6641, .T. ) ;
#7092 = ORIENTED_EDGE ( 'NONE', *, *, #7735, .T. ) ;
#7093 = ORIENTED_EDGE ( 'NONE', *, *, #5715, .T. ) ;
#7094 = UNCERTAINTY_MEASURE_WITH_UNIT (LENGTH_MEASURE( 1.000000000000000082E-05 ), #2964, 'distance_accuracy_value', 'NONE');
#7095 = ORIENTED_EDGE ( 'NONE', *, *, #803, .F. ) ;
#7096 = AXIS2_PLACEMENT_3D ( 'NONE', #7100, #104, #4324 ) ;
#7097 = CYLINDRICAL_SURFACE ( 'NONE', #6315, 150.0000000000000568 ) ;
#7098 = DIRECTION ( 'NONE',  ( -0.000000000000000000, -0.000000000000000000, 1.000000000000000000 ) ) ;
#7099 = DIRECTION ( 'NONE',  ( -1.000000000000000000, 0.000000000000000000, 0.000000000000000000 ) ) ;
#7100 = CARTESIAN_POINT ( 'NONE',  ( -68.76644452187068168, 49.96174644486002592, 10.00000000000000000 ) ) ;
#7101 = VECTOR ( 'NONE', #7058, 1000.000000000000000 ) ;
#7102 = ORIENTED_EDGE ( 'NONE', *, *, #1869, .T. ) ;
#7103 = DIRECTION ( 'NONE',  ( -1.000000000000000000, 0.000000000000000000, 0.000000000000000000 ) ) ;
#7104 = CARTESIAN_POINT ( 'NONE',  ( -5.134781488891348999E-13, 239.9963296805737230, -120.0000000000000000 ) ) ;
#7105 = AXIS2_PLACEMENT_3D ( 'NONE', #2033, #2811, #4427 ) ;
#7106 = LINE ( 'NONE', #6992, #4003 ) ;
#7107 = LINE ( 'NONE', #7067, #7083 ) ;
#7108 = ORIENTED_EDGE ( 'NONE', *, *, #4084, .T. ) ;
#7109 = ORIENTED_EDGE ( 'NONE', *, *, #3750, .T. ) ;
#7110 = COLOUR_RGB ( '',0.8941176470588234615, 0.8941176470588234615, 0.8941176470588234615 ) ;
#7111 = ADVANCED_FACE ( 'NONE', ( #5470 ), #4877, .T. ) ;
#7112 = DIRECTION ( 'NONE',  ( -1.000000000000000000, 0.000000000000000000, 0.000000000000000000 ) ) ;
#7113 = DIRECTION ( 'NONE',  ( 0.000000000000000000, 0.000000000000000000, -1.000000000000000000 ) ) ;
#7114 = CARTESIAN_POINT ( 'NONE',  ( -72.93844452187072136, 49.96174644486006855, -135.0000000000000000 ) ) ;
#7115 = EDGE_CURVE ( 'NONE', #6644, #1120, #7587, .T. ) ;
#7116 = EDGE_CURVE ( 'NONE', #6357, #3312, #5508, .T. ) ;
#7117 = DIRECTION ( 'NONE',  ( 1.000000000000000000, 0.000000000000000000, 0.000000000000000000 ) ) ;
#7118 = CARTESIAN_POINT ( 'NONE',  ( -10.00000000000000000, 41.99999999999999289, -60.00000000000000711 ) ) ;
#7119 = DIRECTION ( 'NONE',  ( -0.000000000000000000, -0.000000000000000000, 1.000000000000000000 ) ) ;
#7120 = ITEM_DEFINED_TRANSFORMATION ( 'NONE', 'NONE', #3596,  #7485 ) ;
#7121 = EDGE_CURVE ( 'NONE', #7440, #5822, #407, .T. ) ;
#7122 = FACE_OUTER_BOUND ( 'NONE', #5188, .T. ) ;
#7123 = ORIENTED_EDGE ( 'NONE', *, *, #1522, .F. ) ;
#7124 =( REPRESENTATION_RELATIONSHIP ('NONE','NONE', #1229, #1433 ) REPRESENTATION_RELATIONSHIP_WITH_TRANSFORMATION ( #7120 )SHAPE_REPRESENTATION_RELATIONSHIP( ) );
#7125 = ORIENTED_EDGE ( 'NONE', *, *, #1183, .T. ) ;
#7126 = ORIENTED_EDGE ( 'NONE', *, *, #7020, .F. ) ;
#7127 = EDGE_CURVE ( 'NONE', #3671, #219, #5834, .T. ) ;
#7128 = DIRECTION ( 'NONE',  ( 1.000000000000000000, 0.000000000000000000, 0.000000000000000000 ) ) ;
#7129 = DIRECTION ( 'NONE',  ( -0.000000000000000000, -0.000000000000000000, 1.000000000000000000 ) ) ;
#7130 = DIRECTION ( 'NONE',  ( 1.000000000000000000, 0.000000000000000000, 0.000000000000000000 ) ) ;
#7131 = AXIS2_PLACEMENT_3D ( 'NONE', #2442, #1356, #1846 ) ;
#7132 = CARTESIAN_POINT ( 'NONE',  ( 0.000000000000000000, 0.000000000000000000, -4.700000000000000178 ) ) ;
#7133 = CARTESIAN_POINT ( 'NONE',  ( 0.000000000000000000, 0.000000000000000000, 10.00000000000000000 ) ) ;
#7134 = VERTEX_POINT ( 'NONE', #7114 ) ;
#7135 = VERTEX_POINT ( 'NONE', #3526 ) ;
#7136 = AXIS2_PLACEMENT_3D ( 'NONE', #4501, #3875, #6802 ) ;
#7137 = ORIENTED_EDGE ( 'NONE', *, *, #7450, .T. ) ;
#7138 = LINE ( 'NONE', #4650, #140 ) ;
#7139 = CARTESIAN_POINT ( 'NONE',  ( 0.000000000000000000, 0.000000000000000000, 2.573333333332999739 ) ) ;
#7140 = FACE_OUTER_BOUND ( 'NONE', #6126, .T. ) ;
#7141 = AXIS2_PLACEMENT_3D ( 'NONE', #7502, #3217, #6329 ) ;
#7142 = ORIENTED_EDGE ( 'NONE', *, *, #5198, .T. ) ;
#7143 = CIRCLE ( 'NONE', #964, 5.250000000000004441 ) ;
#7144 = CARTESIAN_POINT ( 'NONE',  ( 26.26644452187053957, 80.83980388508807380, 10.00000000000000000 ) ) ;
#7145 = FACE_OUTER_BOUND ( 'NONE', #4691, .T. ) ;
#7146 = CARTESIAN_POINT ( 'NONE',  ( -213.0929183184026670, 119.9981648402859378, -50.00000000000000000 ) ) ;
#7147 = CARTESIAN_POINT ( 'NONE',  ( 0.000000000000000000, 0.000000000000000000, -119.9999999999999716 ) ) ;
#7148 = ORIENTED_EDGE ( 'NONE', *, *, #6253, .F. ) ;
#7149 = AXIS2_PLACEMENT_3D ( 'NONE', #996, #3489, #2861 ) ;
#7150 = VERTEX_POINT ( 'NONE', #3382 ) ;
#7151 = ORIENTED_EDGE ( 'NONE', *, *, #3974, .F. ) ;
#7152 = DIRECTION ( 'NONE',  ( -0.000000000000000000, -0.000000000000000000, 1.000000000000000000 ) ) ;
#7153 = DIRECTION ( 'NONE',  ( -0.8571673007021121116, 1.049727191138618449E-16, 0.5150380749100544886 ) ) ;
#7154 = AXIS2_PLACEMENT_3D ( 'NONE', #1944, #5967, #1381 ) ;
#7155 = DIRECTION ( 'NONE',  ( -0.9914631140645256968, 0.1303874742813643794, 0.000000000000000000 ) ) ;
#7156 = CARTESIAN_POINT ( 'NONE',  ( -58.76644452187068168, 49.96174644486002592, -40.00000000000000000 ) ) ;
#7157 = DIRECTION ( 'NONE',  ( -1.000000000000000000, 0.000000000000000000, 0.000000000000000000 ) ) ;
#7158 = CONTEXT_DEPENDENT_SHAPE_REPRESENTATION ( #3492, #3095 ) ;
#7159 = DIRECTION ( 'NONE',  ( 0.000000000000000000, 0.000000000000000000, 1.000000000000000000 ) ) ;
#7160 = VERTEX_POINT ( 'NONE', #4785 ) ;
#7161 = ORIENTED_EDGE ( 'NONE', *, *, #573, .T. ) ;
#7162 = AXIS2_PLACEMENT_3D ( 'NONE', #6426, #162, #7638 ) ;
#7163 = EDGE_CURVE ( 'NONE', #3939, #6450, #2328, .T. ) ;
#7164 = CARTESIAN_POINT ( 'NONE',  ( -4.000000000000004441, 6.928203230275506108, -4.700000000000000178 ) ) ;
#7165 = CIRCLE ( 'NONE', #484, 35.00000000000000711 ) ;
#7166 = LINE ( 'NONE', #4318, #2885 ) ;
#7167 = DIRECTION ( 'NONE',  ( 0.9938725510941108787, -0.1105321318969463978, 0.000000000000000000 ) ) ;
#7168 = DIRECTION ( 'NONE',  ( -0.8090169943749422332, -0.5877852522924802425, 0.000000000000000000 ) ) ;
#7169 = APPLICATION_CONTEXT ( 'automotive_design' ) ;
#7170 = CYLINDRICAL_SURFACE ( 'NONE', #3709, 0.7500000000000041078 ) ;
#7171 = CARTESIAN_POINT ( 'NONE',  ( -119.9981648402868046, 207.8429183184021554, -8.673617379884035472E-15 ) ) ;
#7172 = ADVANCED_FACE ( 'NONE', ( #1113 ), #283, .T. ) ;
#7173 = ORIENTED_EDGE ( 'NONE', *, *, #5323, .T. ) ;
#7174 = CIRCLE ( 'NONE', #5024, 150.0000000000000568 ) ;
#7175 = EDGE_LOOP ( 'NONE', ( #1737, #2424, #1130, #2130 ) ) ;
#7176 = EDGE_CURVE ( 'NONE', #3469, #1337, #2449, .T. ) ;
#7177 = ORIENTED_EDGE ( 'NONE', *, *, #426, .F. ) ;
#7178 = FACE_OUTER_BOUND ( 'NONE', #1063, .T. ) ;
#7179 = PLANE ( 'NONE',  #5027 ) ;
#7180 = VECTOR ( 'NONE', #3188, 1000.000000000000000 ) ;
#7181 = LINE ( 'NONE', #5999, #6854 ) ;
#7182 = EDGE_CURVE ( 'NONE', #2329, #1610, #5457, .T. ) ;
#7183 = PRODUCT_DEFINITION_SHAPE ( 'NONE', 'NONE',  #7786 ) ;
#7184 = EDGE_LOOP ( 'NONE', ( #3586, #5349, #3072, #2148 ) ) ;
#7185 = EDGE_LOOP ( 'NONE', ( #6910, #278, #6462, #7053 ) ) ;
#7186 = CIRCLE ( 'NONE', #1507, 30.00000000000000355 ) ;
#7187 = EDGE_CURVE ( 'NONE', #1561, #1335, #376, .T. ) ;
#7188 = CYLINDRICAL_SURFACE ( 'NONE', #3791, 37.49999999999997868 ) ;
#7189 = CARTESIAN_POINT ( 'NONE',  ( -145.1064334105735725, 38.00161816110973234, 5.000000000000000000 ) ) ;
#7190 = AXIS2_PLACEMENT_3D ( 'NONE', #514, #3556, #5372 ) ;
#7191 = DIRECTION ( 'NONE',  ( -0.000000000000000000, -0.000000000000000000, 1.000000000000000000 ) ) ;
#7192 = ORIENTED_EDGE ( 'NONE', *, *, #2590, .T. ) ;
#7193 = EDGE_LOOP ( 'NONE', ( #6905, #6155 ) ) ;
#7194 = EDGE_LOOP ( 'NONE', ( #710, #5200, #5058, #5440 ) ) ;
#7195 = AXIS2_PLACEMENT_3D ( 'NONE', #2418, #3117, #3630 ) ;
#7196 = DIRECTION ( 'NONE',  ( 1.000000000000000000, 0.000000000000000000, 0.000000000000000000 ) ) ;
#7197 = DIRECTION ( 'NONE',  ( -0.000000000000000000, -0.000000000000000000, 1.000000000000000000 ) ) ;
#7198 = FACE_BOUND ( 'NONE', #4743, .T. ) ;
#7199 = DIRECTION ( 'NONE',  ( -0.000000000000000000, -0.000000000000000000, -1.000000000000000000 ) ) ;
#7200 = CONTEXT_DEPENDENT_SHAPE_REPRESENTATION ( #5205, #694 ) ;
#7201 = LINE ( 'NONE', #3023, #5949 ) ;
#7202 = ORIENTED_EDGE ( 'NONE', *, *, #7082, .F. ) ;
#7203 = ORIENTED_EDGE ( 'NONE', *, *, #6939, .T. ) ;
#7204 = EDGE_CURVE ( 'NONE', #6340, #3290, #7721, .T. ) ;
#7205 = LINE ( 'NONE', #1808, #6758 ) ;
#7206 = DIRECTION ( 'NONE',  ( 0.000000000000000000, 0.000000000000000000, 1.000000000000000000 ) ) ;
#7207 = DIRECTION ( 'NONE',  ( 0.000000000000000000, 0.000000000000000000, 1.000000000000000000 ) ) ;
#7208 = CARTESIAN_POINT ( 'NONE',  ( 207.8429183184021838, 119.9981648402868188, -124.7000000000000028 ) ) ;
#7209 = LINE ( 'NONE', #3624, #2770 ) ;
#7210 = ORIENTED_EDGE ( 'NONE', *, *, #94, .F. ) ;
#7211 = VECTOR ( 'NONE', #1274, 1000.000000000000000 ) ;
#7212 = ORIENTED_EDGE ( 'NONE', *, *, #894, .T. ) ;
#7213 = EDGE_CURVE ( 'NONE', #5950, #6794, #5705, .T. ) ;
#7214 = ORIENTED_EDGE ( 'NONE', *, *, #6879, .T. ) ;
#7215 = LINE ( 'NONE', #703, #4541 ) ;
#7216 = DIRECTION ( 'NONE',  ( -1.000000000000000000, 0.000000000000000000, 0.000000000000000000 ) ) ;
#7217 = EDGE_CURVE ( 'NONE', #7619, #3392, #787, .T. ) ;
#7218 = CIRCLE ( 'NONE', #1934, 37.49999999999997868 ) ;
#7219 = EDGE_CURVE ( 'NONE', #4399, #1948, #3969, .T. ) ;
#7220 = UNCERTAINTY_MEASURE_WITH_UNIT (LENGTH_MEASURE( 1.000000000000000082E-05 ), #6776, 'distance_accuracy_value', 'NONE');
#7221 = PRODUCT_DEFINITION_FORMATION_WITH_SPECIFIED_SOURCE ( 'ANY', '', #7248, .NOT_KNOWN. ) ;
#7222 = FACE_OUTER_BOUND ( 'NONE', #1805, .T. ) ;
#7223 = EDGE_CURVE ( 'NONE', #5511, #6752, #6463, .T. ) ;
#7224 = EDGE_LOOP ( 'NONE', ( #4596, #4611, #1940, #663 ) ) ;
#7225 = ORIENTED_EDGE ( 'NONE', *, *, #4415, .T. ) ;
#7226 = EDGE_CURVE ( 'NONE', #3552, #1582, #3019, .T. ) ;
#7227 = DIRECTION ( 'NONE',  ( 0.000000000000000000, 0.000000000000000000, 1.000000000000000000 ) ) ;
#7228 = EDGE_CURVE ( 'NONE', #2154, #5950, #2754, .T. ) ;
#7229 = DIRECTION ( 'NONE',  ( 1.000000000000000000, 0.000000000000000000, 0.000000000000000000 ) ) ;
#7230 = CIRCLE ( 'NONE', #5079, 30.00000000000000000 ) ;
#7231 = DIRECTION ( 'NONE',  ( -0.000000000000000000, -0.000000000000000000, 1.000000000000000000 ) ) ;
#7232 = VERTEX_POINT ( 'NONE', #2433 ) ;
#7233 = VERTEX_POINT ( 'NONE', #5744 ) ;
#7234 = AXIS2_PLACEMENT_3D ( 'NONE', #3541, #1167, #4010 ) ;
#7235 = VECTOR ( 'NONE', #4579, 1000.000000000000000 ) ;
#7236 = CARTESIAN_POINT ( 'NONE',  ( 0.000000000000000000, 0.000000000000000000, -82.99999999999998579 ) ) ;
#7237 = FACE_OUTER_BOUND ( 'NONE', #1363, .T. ) ;
#7238 = FACE_OUTER_BOUND ( 'NONE', #7763, .T. ) ;
#7239 = FACE_BOUND ( 'NONE', #774, .T. ) ;
#7240 = CARTESIAN_POINT ( 'NONE',  ( -0.5700000000000001732, -28.49429942988597020, 0.000000000000000000 ) ) ;
#7241 = COLOUR_RGB ( '',0.8941176470588234615, 0.8941176470588234615, 0.8941176470588234615 ) ;
#7242 = ORIENTED_EDGE ( 'NONE', *, *, #6395, .T. ) ;
#7243 = MECHANICAL_DESIGN_GEOMETRIC_PRESENTATION_REPRESENTATION (  '', ( #5849 ), #6360 ) ;
#7244 = LINE ( 'NONE', #6689, #157 ) ;
#7245 = CARTESIAN_POINT ( 'NONE',  ( -5.250000000000505374, 239.9963296805737230, -50.00000000000000000 ) ) ;
#7246 = DIRECTION ( 'NONE',  ( 1.000000000000000000, -1.586032892321652482E-16, 0.000000000000000000 ) ) ;
#7247 = DIRECTION ( 'NONE',  ( 0.3334338027881733613, 0.9427735142430646587, 1.931932416011734352E-18 ) ) ;
#7248 = PRODUCT ( 'angular contact ball bearing_68_iso_ISO 15 ABB - 1760 - 38,SI,NC,38_68', 'angular contact ball bearing_68_iso_ISO 15 ABB - 1760 - 38,SI,NC,38_68', '', ( #6256 ) ) ;
#7249 =( NAMED_UNIT ( * ) SI_UNIT ( $, .STERADIAN. ) SOLID_ANGLE_UNIT ( ) );
#7250 = CARTESIAN_POINT ( 'NONE',  ( 8.000000000000000000, 0.000000000000000000, 9.480888224575629408 ) ) ;
#7251 = FACE_OUTER_BOUND ( 'NONE', #3603, .T. ) ;
#7252 = ORIENTED_EDGE ( 'NONE', *, *, #5713, .T. ) ;
#7253 = AXIS2_PLACEMENT_3D ( 'NONE', #2445, #4833, #7247 ) ;
#7254 = EDGE_LOOP ( 'NONE', ( #937, #3984, #6820, #5227 ) ) ;
#7255 = ORIENTED_EDGE ( 'NONE', *, *, #7401, .F. ) ;
#7256 = DIRECTION ( 'NONE',  ( 1.000000000000000000, 0.000000000000000000, 0.000000000000000000 ) ) ;
#7257 = CARTESIAN_POINT ( 'NONE',  ( -5.846731056662405557, 29.42474699893032053, -79.99999999999995737 ) ) ;
#7258 = SHAPE_REPRESENTATION_RELATIONSHIP ( 'NONE' , 'NONE' ,  #1433, #7262 ) ;
#7259 = LINE ( 'NONE', #4370, #1049 ) ;
#7260 = VERTEX_POINT ( 'NONE', #4823 ) ;
#7261 = ORIENTED_EDGE ( 'NONE', *, *, #4183, .F. ) ;
#7262 = ADVANCED_BREP_SHAPE_REPRESENTATION ( '', ( #3145, #7485 ), #309 ) ;
#7263 = ADVANCED_FACE ( 'NONE', ( #7237 ), #7592, .F. ) ;
#7264 = CARTESIAN_POINT ( 'NONE',  ( 9.702951051037011609, -29.86427928513813868, 0.000000000000000000 ) ) ;
#7265 = CIRCLE ( 'NONE', #3866, 32.25000000000000000 ) ;
#7266 = CARTESIAN_POINT ( 'NONE',  ( -0.6543471694412565931, -8.859816792613647962, -0.4964154566687977721 ) ) ;
#7267 = DIRECTION ( 'NONE',  ( 1.000000000000000000, 0.000000000000000000, -0.000000000000000000 ) ) ;
#7268 = ORIENTED_EDGE ( 'NONE', *, *, #1084, .T. ) ;
#7269 = EDGE_CURVE ( 'NONE', #2058, #1947, #5152, .T. ) ;
#7270 = VECTOR ( 'NONE', #1028, 1000.000000000000000 ) ;
#7271 = EDGE_LOOP ( 'NONE', ( #5417, #6298, #2165, #7487 ) ) ;
#7272 =( REPRESENTATION_RELATIONSHIP ('NONE','NONE', #1229, #1433 ) REPRESENTATION_RELATIONSHIP_WITH_TRANSFORMATION ( #5345 )SHAPE_REPRESENTATION_RELATIONSHIP( ) );
#7273 = CYLINDRICAL_SURFACE ( 'NONE', #7633, 5.249999999999976907 ) ;
#7274 = FACE_OUTER_BOUND ( 'NONE', #4372, .T. ) ;
#7275 = DIRECTION ( 'NONE',  ( -1.000000000000000000, 0.000000000000000000, 0.000000000000000000 ) ) ;
#7276 = CARTESIAN_POINT ( 'NONE',  ( 3.716043017018883621, 28.25669875083898930, 10.00000000000000000 ) ) ;
#7277 = CONTEXT_DEPENDENT_SHAPE_REPRESENTATION ( #117, #5611 ) ;
#7278 = AXIS2_PLACEMENT_3D ( 'NONE', #6539, #1774, #5988 ) ;
#7279 = CARTESIAN_POINT ( 'NONE',  ( 279.9963296805736945, -6.783120157456498832E-12, 0.000000000000000000 ) ) ;
#7280 = ORIENTED_EDGE ( 'NONE', *, *, #3497, .F. ) ;
#7281 = CARTESIAN_POINT ( 'NONE',  ( -1.852913429037944315, 300.0000000000000568, -82.99999999999998579 ) ) ;
#7282 = ADVANCED_FACE ( 'NONE', ( #2169 ), #5196, .T. ) ;
#7283 = FACE_OUTER_BOUND ( 'NONE', #5701, .T. ) ;
#7284 = CARTESIAN_POINT ( 'NONE',  ( -105.4635834177236546, -106.6650485055571380, 0.000000000000000000 ) ) ;
#7285 = CARTESIAN_POINT ( 'NONE',  ( -42.49999999999948841, 166.3841703588958296, 0.000000000000000000 ) ) ;
#7286 = DIRECTION ( 'NONE',  ( 0.1305261922200541547, -0.9914448613738101601, 0.000000000000000000 ) ) ;
#7287 = DIRECTION ( 'NONE',  ( 0.000000000000000000, 0.000000000000000000, -1.000000000000000000 ) ) ;
#7288 = UNCERTAINTY_MEASURE_WITH_UNIT (LENGTH_MEASURE( 1.000000000000000082E-05 ), #3548, 'distance_accuracy_value', 'NONE');
#7289 = CARTESIAN_POINT ( 'NONE',  ( 0.5700000000000001732, -28.49429942988597020, -3.000000000000000000 ) ) ;
#7290 = AXIS2_PLACEMENT_3D ( 'NONE', #3249, #6325, #5095 ) ;
#7291 = VERTEX_POINT ( 'NONE', #6566 ) ;
#7292 = ORIENTED_EDGE ( 'NONE', *, *, #5326, .T. ) ;
#7293 = CIRCLE ( 'NONE', #2261, 37.50000000000000000 ) ;
#7294 = ORIENTED_EDGE ( 'NONE', *, *, #7310, .F. ) ;
#7295 = CARTESIAN_POINT ( 'NONE',  ( 199.9963296805737230, -4.860399174643270382E-12, 0.000000000000000000 ) ) ;
#7296 = DIRECTION ( 'NONE',  ( 0.9412010056177179118, 0.3378471059875997051, 0.000000000000000000 ) ) ;
#7297 = PRESENTATION_STYLE_ASSIGNMENT (( #3 ) ) ;
#7298 = DIRECTION ( 'NONE',  ( 1.000000000000000000, 0.000000000000000000, 0.000000000000000000 ) ) ;
#7299 = CIRCLE ( 'NONE', #1499, 32.81578194438969120 ) ;
#7300 = ORIENTED_EDGE ( 'NONE', *, *, #7647, .F. ) ;
#7301 = ORIENTED_EDGE ( 'NONE', *, *, #2684, .T. ) ;
#7302 = AXIS2_PLACEMENT_3D ( 'NONE', #3695, #2006, #2524 ) ;
#7303 = ADVANCED_FACE ( 'NONE', ( #3566, #2396 ), #6803, .T. ) ;
#7304 = CARTESIAN_POINT ( 'NONE',  ( -11.50644898236017433, -35.69105814929478981, -3.000000000000000000 ) ) ;
#7305 = CARTESIAN_POINT ( 'NONE',  ( 32.81578194438969120, 1.484218055610305731, -3.000000000000000000 ) ) ;
#7306 = CARTESIAN_POINT ( 'NONE',  ( -10.00000000000000000, 33.54101966249685773, -50.00000000000000000 ) ) ;
#7307 = VERTEX_POINT ( 'NONE', #1389 ) ;
#7308 = ORIENTED_EDGE ( 'NONE', *, *, #5237, .T. ) ;
#7309 = PRODUCT_DEFINITION_SHAPE ( 'NONE', 'NONE',  #4161 ) ;
#7310 = EDGE_CURVE ( 'NONE', #2413, #1191, #3948, .T. ) ;
#7311 = DIRECTION ( 'NONE',  ( -0.000000000000000000, -0.000000000000000000, 1.000000000000000000 ) ) ;
#7312 = FACE_OUTER_BOUND ( 'NONE', #106, .T. ) ;
#7313 = CIRCLE ( 'NONE', #4661, 150.0000000000000568 ) ;
#7314 = DIRECTION ( 'NONE',  ( -1.000000000000000000, 0.000000000000000000, 0.000000000000000000 ) ) ;
#7315 = DIRECTION ( 'NONE',  ( 0.000000000000000000, 0.000000000000000000, 1.000000000000000000 ) ) ;
#7316 = ADVANCED_FACE ( 'NONE', ( #7424 ), #1550, .F. ) ;
#7317 = EDGE_CURVE ( 'NONE', #4191, #6073, #4953, .T. ) ;
#7318 = UNCERTAINTY_MEASURE_WITH_UNIT (LENGTH_MEASURE( 1.000000000000000082E-05 ), #4479, 'distance_accuracy_value', 'NONE');
#7319 = FACE_OUTER_BOUND ( 'NONE', #6158, .T. ) ;
#7320 = VERTEX_POINT ( 'NONE', #3137 ) ;
#7321 = ADVANCED_FACE ( 'NONE', ( #7312 ), #5570, .T. ) ;
#7322 = AXIS2_PLACEMENT_3D ( 'NONE', #495, #1163, #7047 ) ;
#7323 = CYLINDRICAL_SURFACE ( 'NONE', #5559, 40.00000000000000711 ) ;
#7324 = ADVANCED_FACE ( 'NONE', ( #6090 ), #3098, .T. ) ;
#7325 = CARTESIAN_POINT ( 'NONE',  ( 125.2481648402866199, 207.8429183184022122, -120.0000000000000000 ) ) ;
#7326 = DIRECTION ( 'NONE',  ( -0.000000000000000000, -0.000000000000000000, 1.000000000000000000 ) ) ;
#7327 = SHAPE_DEFINITION_REPRESENTATION ( #6244, #1433 ) ;
#7328 = AXIS2_PLACEMENT_3D ( 'NONE', #7404, #3271, #2675 ) ;
#7329 = LINE ( 'NONE', #5589, #868 ) ;
#7330 = CARTESIAN_POINT ( 'NONE',  ( 0.000000000000000000, 0.000000000000000000, 10.00000000000000000 ) ) ;
#7331 = EDGE_CURVE ( 'NONE', #1947, #7551, #6846, .T. ) ;
#7332 = ORIENTED_EDGE ( 'NONE', *, *, #1677, .T. ) ;
#7333 = ORIENTED_EDGE ( 'NONE', *, *, #5631, .T. ) ;
#7334 = ORIENTED_EDGE ( 'NONE', *, *, #94, .T. ) ;
#7335 = DIRECTION ( 'NONE',  ( 0.000000000000000000, -0.000000000000000000, -1.000000000000000000 ) ) ;
#7336 = CARTESIAN_POINT ( 'NONE',  ( 5.000000000000000888, 6.123233995736767268E-16, -4.674599999999997202 ) ) ;
#7337 = ORIENTED_EDGE ( 'NONE', *, *, #5473, .F. ) ;
#7338 = VERTEX_POINT ( 'NONE', #721 ) ;
#7339 = ORIENTED_EDGE ( 'NONE', *, *, #512, .F. ) ;
#7340 = CIRCLE ( 'NONE', #4812, 4.250000000000000000 ) ;
#7341 = ORIENTED_EDGE ( 'NONE', *, *, #2224, .F. ) ;
#7342 = CARTESIAN_POINT ( 'NONE',  ( -64.59444452187072727, 49.96174644486006855, -135.0000000000000000 ) ) ;
#7343 = DIRECTION ( 'NONE',  ( 0.1303874742813643517, 0.9914631140645255858, 0.000000000000000000 ) ) ;
#7344 = DIRECTION ( 'NONE',  ( 1.000000000000000000, 0.000000000000000000, 0.000000000000000000 ) ) ;
#7345 = CARTESIAN_POINT ( 'NONE',  ( 3.319543390096037605, -7.321065037175434220, -0.01688885742777183549 ) ) ;
#7346 = VERTEX_POINT ( 'NONE', #3803 ) ;
#7347 = ORIENTED_EDGE ( 'NONE', *, *, #1968, .F. ) ;
#7348 = CARTESIAN_POINT ( 'NONE',  ( -199.9963296805737230, 0.000000000000000000, 10.00000000000000000 ) ) ;
#7349 = CARTESIAN_POINT ( 'NONE',  ( 2.583028308771596837, 28.38270538120150377, 10.00000000000000000 ) ) ;
#7350 = AXIS2_PLACEMENT_3D ( 'NONE', #5382, #6380, #1714 ) ;
#7351 = CARTESIAN_POINT ( 'NONE',  ( 0.000000000000000000, 0.000000000000000000, -50.00000000000000000 ) ) ;
#7352 = CARTESIAN_POINT ( 'NONE',  ( -8.000000000000000000, 4.618802153517003184, -4.700000000000000178 ) ) ;
#7353 = CARTESIAN_POINT ( 'NONE',  ( -68.76644452187024115, -49.96174644486060856, 10.00000000000000000 ) ) ;
#7354 = ORIENTED_EDGE ( 'NONE', *, *, #560, .T. ) ;
#7355 = EDGE_CURVE ( 'NONE', #7016, #2430, #3057, .T. ) ;
#7356 = AXIS2_PLACEMENT_3D ( 'NONE', #7489, #4496, #943 ) ;
#7357 = EDGE_CURVE ( 'NONE', #3615, #6864, #3711, .T. ) ;
#7358 = DIRECTION ( 'NONE',  ( 1.000000000000000000, 0.000000000000000000, 0.000000000000000000 ) ) ;
#7359 = EDGE_CURVE ( 'NONE', #5872, #1401, #3833, .T. ) ;
#7360 = CARTESIAN_POINT ( 'NONE',  ( 129.9038105676649764, 75.00000000000153477, 10.00000000000000000 ) ) ;
#7361 = DIRECTION ( 'NONE',  ( -0.000000000000000000, -0.000000000000000000, 1.000000000000000000 ) ) ;
#7362 = CIRCLE ( 'NONE', #6604, 279.9963296805736945 ) ;
#7363 = AXIS2_PLACEMENT_3D ( 'NONE', #2124, #6957, #366 ) ;
#7364 = LINE ( 'NONE', #3109, #2831 ) ;
#7365 = DIRECTION ( 'NONE',  ( 1.000000000000000000, 0.000000000000000000, 0.000000000000000000 ) ) ;
#7366 = CARTESIAN_POINT ( 'NONE',  ( 0.000000000000000000, 0.000000000000000000, 10.00000000000000000 ) ) ;
#7367 = ORIENTED_EDGE ( 'NONE', *, *, #81, .T. ) ;
#7368 = VERTEX_POINT ( 'NONE', #683 ) ;
#7369 = EDGE_CURVE ( 'NONE', #1526, #989, #6605, .T. ) ;
#7370 = CIRCLE ( 'NONE', #5218, 32.49999999999997158 ) ;
#7371 = ORIENTED_EDGE ( 'NONE', *, *, #7412, .T. ) ;
#7372 = B_SPLINE_CURVE_WITH_KNOTS ( 'NONE', 3,
 ( #3052, #7266, #1865, #4262, #4894, #3675 ),
 .UNSPECIFIED., .F., .F.,
 ( 4, 2, 4 ),
 ( 2.380731629811925857E-07, 0.002336973833157575484, 0.004673709593152171327 ),
 .UNSPECIFIED. ) ;
#7373 = DIRECTION ( 'NONE',  ( -0.000000000000000000, -0.000000000000000000, 1.000000000000000000 ) ) ;
#7374 = DIRECTION ( 'NONE',  ( 5.551115123125782702E-17, 0.000000000000000000, 1.000000000000000000 ) ) ;
#7375 =( GEOMETRIC_REPRESENTATION_CONTEXT ( 3 ) GLOBAL_UNCERTAINTY_ASSIGNED_CONTEXT ( ( #7094 ) ) GLOBAL_UNIT_ASSIGNED_CONTEXT ( ( #2964, #6587, #112 ) ) REPRESENTATION_CONTEXT ( 'NONE', 'WORKASPACE' ) );
#7376 = EDGE_LOOP ( 'NONE', ( #7354, #4994 ) ) ;
#7377 = ORIENTED_EDGE ( 'NONE', *, *, #946, .T. ) ;
#7378 = EDGE_LOOP ( 'NONE', ( #1221, #1590, #7332, #1757 ) ) ;
#7379 = CARTESIAN_POINT ( 'NONE',  ( 0.000000000000000000, 0.000000000000000000, 0.000000000000000000 ) ) ;
#7380 = DIRECTION ( 'NONE',  ( 0.000000000000000000, -1.000000000000000000, 0.000000000000000000 ) ) ;
#7381 = CARTESIAN_POINT ( 'NONE',  ( 1.310872448937991486, -8.480771745766411129, -0.3173508448886628863 ) ) ;
#7382 = EDGE_LOOP ( 'NONE', ( #6675, #5339, #7668, #6314 ) ) ;
#7383 = CIRCLE ( 'NONE', #953, 5.000000000000004441 ) ;
#7384 = CARTESIAN_POINT ( 'NONE',  ( -0.5700000000000001732, -28.49429942988597020, -3.000000000000000000 ) ) ;
#7385 = CARTESIAN_POINT ( 'NONE',  ( 0.000000000000000000, 0.000000000000000000, -50.00000000000000000 ) ) ;
#7386 = DIRECTION ( 'NONE',  ( -1.000000000000000000, 2.403401228516536636E-14, 0.000000000000000000 ) ) ;
#7387 = UNCERTAINTY_MEASURE_WITH_UNIT (LENGTH_MEASURE( 1.000000000000000082E-05 ), #1979, 'distance_accuracy_value', 'NONE');
#7388 = DIRECTION ( 'NONE',  ( 1.000000000000000000, 0.000000000000000000, 0.000000000000000000 ) ) ;
#7389 = VERTEX_POINT ( 'NONE', #645 ) ;
#7390 = AXIS2_PLACEMENT_3D ( 'NONE', #2591, #4508, #1354 ) ;
#7391 = FACE_BOUND ( 'NONE', #2038, .T. ) ;
#7392 = DIRECTION ( 'NONE',  ( 0.000000000000000000, 0.000000000000000000, -1.000000000000000000 ) ) ;
#7393 = AXIS2_PLACEMENT_3D ( 'NONE', #4590, #3962, #6888 ) ;
#7394 = PRODUCT_DEFINITION ( 'UNKNOWN', '', #5957, #2986 ) ;
#7395 = CARTESIAN_POINT ( 'NONE',  ( 4.586480920263560357, -37.21846574978686562, -3.000000000000000000 ) ) ;
#7396 = FACE_OUTER_BOUND ( 'NONE', #7194, .T. ) ;
#7397 = CYLINDRICAL_SURFACE ( 'NONE', #7302, 37.50000000000000000 ) ;
#7398 = VERTEX_POINT ( 'NONE', #133 ) ;
#7399 = ORIENTED_EDGE ( 'NONE', *, *, #4415, .F. ) ;
#7400 = VECTOR ( 'NONE', #7386, 1000.000000000000000 ) ;
#7401 = EDGE_CURVE ( 'NONE', #1496, #4531, #4713, .T. ) ;
#7402 = ORIENTED_EDGE ( 'NONE', *, *, #7116, .T. ) ;
#7403 = ORIENTED_EDGE ( 'NONE', *, *, #122, .F. ) ;
#7404 = CARTESIAN_POINT ( 'NONE',  ( -68.76644452187072432, 49.96174644486006855, -40.00000000000000000 ) ) ;
#7405 = SURFACE_STYLE_USAGE ( .BOTH. , #1406 ) ;
#7406 =( LENGTH_UNIT ( ) NAMED_UNIT ( * ) SI_UNIT ( .MILLI., .METRE. ) );
#7407 = CIRCLE ( 'NONE', #5520, 29.99999999999999289 ) ;
#7408 = LINE ( 'NONE', #2137, #5717 ) ;
#7409 = EDGE_CURVE ( 'NONE', #6843, #5609, #800, .T. ) ;
#7410 = ORIENTED_EDGE ( 'NONE', *, *, #4893, .F. ) ;
#7411 = AXIS2_PLACEMENT_3D ( 'NONE', #3853, #3222, #2043 ) ;
#7412 = EDGE_CURVE ( 'NONE', #2088, #3277, #4861, .T. ) ;
#7413 = VERTEX_POINT ( 'NONE', #6172 ) ;
#7414 = AXIS2_PLACEMENT_3D ( 'NONE', #5236, #5274, #541 ) ;
#7415 = DIRECTION ( 'NONE',  ( 0.000000000000000000, 0.000000000000000000, 1.000000000000000000 ) ) ;
#7416 = AXIS2_PLACEMENT_3D ( 'NONE', #2742, #6412, #6371 ) ;
#7417 = ADVANCED_FACE ( 'NONE', ( #7274 ), #4386, .F. ) ;
#7418 = LINE ( 'NONE', #3831, #3387 ) ;
#7419 = APPLICATION_CONTEXT ( 'automotive_design' ) ;
#7420 = LINE ( 'NONE', #6799, #2808 ) ;
#7421 = EDGE_LOOP ( 'NONE', ( #3491, #825, #781, #2093 ) ) ;
#7422 = ADVANCED_FACE ( 'NONE', ( #5019 ), #4232, .T. ) ;
#7423 = CIRCLE ( 'NONE', #7046, 37.49999999999997868 ) ;
#7424 = FACE_OUTER_BOUND ( 'NONE', #4856, .T. ) ;
#7425 = FACE_OUTER_BOUND ( 'NONE', #7175, .T. ) ;
#7426 =( GEOMETRIC_REPRESENTATION_CONTEXT ( 3 ) GLOBAL_UNCERTAINTY_ASSIGNED_CONTEXT ( ( #6611 ) ) GLOBAL_UNIT_ASSIGNED_CONTEXT ( ( #1895, #4294, #6112 ) ) REPRESENTATION_CONTEXT ( 'NONE', 'WORKASPACE' ) );
#7427 = DIRECTION ( 'NONE',  ( 0.000000000000000000, 0.000000000000000000, -1.000000000000000000 ) ) ;
#7428 = EDGE_LOOP ( 'NONE', ( #3055, #2118, #1493, #5910 ) ) ;
#7429 = CARTESIAN_POINT ( 'NONE',  ( 0.3344772040064616925, 4.088789500653224965E-15, -31.52499999999999858 ) ) ;
#7430 = AXIS2_PLACEMENT_3D ( 'NONE', #3201, #2764, #5009 ) ;
#7431 = CARTESIAN_POINT ( 'NONE',  ( 0.000000000000000000, 0.000000000000000000, -82.99999999999998579 ) ) ;
#7432 = DIRECTION ( 'NONE',  ( -0.000000000000000000, -0.000000000000000000, 1.000000000000000000 ) ) ;
#7433 = DIRECTION ( 'NONE',  ( -0.000000000000000000, -0.000000000000000000, 1.000000000000000000 ) ) ;
#7434 = APPLICATION_PROTOCOL_DEFINITION ( 'draft international standard', 'automotive_design', 1998, #567 ) ;
#7435 = PRODUCT_DEFINITION_SHAPE ( 'NONE', 'NONE',  #302 ) ;
#7436 = CARTESIAN_POINT ( 'NONE',  ( 0.000000000000000000, 0.000000000000000000, -139.9999999999999716 ) ) ;
#7437 = DIRECTION ( 'NONE',  ( 1.000000000000000000, 0.000000000000000000, 0.000000000000000000 ) ) ;
#7438 = ORIENTED_EDGE ( 'NONE', *, *, #4029, .T. ) ;
#7439 = ORIENTED_EDGE ( 'NONE', *, *, #1580, .F. ) ;
#7440 = VERTEX_POINT ( 'NONE', #3912 ) ;
#7441 = ORIENTED_EDGE ( 'NONE', *, *, #6398, .T. ) ;
#7442 = AXIS2_PLACEMENT_3D ( 'NONE', #6665, #6076, #664 ) ;
#7443 = FACE_OUTER_BOUND ( 'NONE', #6347, .T. ) ;
#7444 = LINE ( 'NONE', #1006, #6676 ) ;
#7445 = FILL_AREA_STYLE_COLOUR ( '', #6989 ) ;
#7446 = FACE_OUTER_BOUND ( 'NONE', #2906, .T. ) ;
#7447 = VERTEX_POINT ( 'NONE', #948 ) ;
#7448 = EDGE_CURVE ( 'NONE', #7150, #989, #4968, .T. ) ;
#7449 = EDGE_LOOP ( 'NONE', ( #4849, #3703 ) ) ;
#7450 = EDGE_CURVE ( 'NONE', #7260, #5121, #5843, .T. ) ;
#7451 = EDGE_CURVE ( 'NONE', #3050, #3424, #275, .T. ) ;
#7452 = CARTESIAN_POINT ( 'NONE',  ( -78.76644452187068168, 49.96174644486002592, -40.00000000000000000 ) ) ;
#7453 = PRESENTATION_STYLE_ASSIGNMENT (( #2143 ) ) ;
#7454 = EDGE_CURVE ( 'NONE', #1043, #3634, #5213, .T. ) ;
#7455 = CYLINDRICAL_SURFACE ( 'NONE', #5405, 28.50000000000000355 ) ;
#7456 = CARTESIAN_POINT ( 'NONE',  ( 9.090232026328989079, -27.01143612819398143, -122.9999999999999716 ) ) ;
#7457 = ORIENTED_EDGE ( 'NONE', *, *, #7317, .F. ) ;
#7458 = CIRCLE ( 'NONE', #2678, 30.00000000000000355 ) ;
#7459 = EDGE_CURVE ( 'NONE', #57, #4452, #3988, .T. ) ;
#7460 = DIRECTION ( 'NONE',  ( -1.000000000000000000, -0.000000000000000000, -0.000000000000000000 ) ) ;
#7461 = CARTESIAN_POINT ( 'NONE',  ( 0.000000000000000000, 0.000000000000000000, 10.00000000000000000 ) ) ;
#7462 = CARTESIAN_POINT ( 'NONE',  ( 0.000000000000000000, 0.000000000000000000, 2.573333333332999739 ) ) ;
#7463 = AXIS2_PLACEMENT_3D ( 'NONE', #1990, #4381, #1416 ) ;
#7464 = AXIS2_PLACEMENT_3D ( 'NONE', #6728, #4438, #179 ) ;
#7465 = CARTESIAN_POINT ( 'NONE',  ( -68.76644452187068168, 49.96174644486002592, 0.000000000000000000 ) ) ;
#7466 = ORIENTED_EDGE ( 'NONE', *, *, #565, .T. ) ;
#7467 = FACE_BOUND ( 'NONE', #1254, .T. ) ;
#7468 = AXIS2_PLACEMENT_3D ( 'NONE', #3983, #7529, #5798 ) ;
#7469 = CYLINDRICAL_SURFACE ( 'NONE', #949, 30.00000000000000000 ) ;
#7470 = CARTESIAN_POINT ( 'NONE',  ( -4.432034252711344102, 28.15327818181735964, -82.99999999999995737 ) ) ;
#7471 = DIRECTION ( 'NONE',  ( 1.000000000000000000, 0.000000000000000000, 0.000000000000000000 ) ) ;
#7472 = SHAPE_DEFINITION_REPRESENTATION ( #7435, #7725 ) ;
#7473 = FILL_AREA_STYLE ('',( #6335 ) ) ;
#7474 = VECTOR ( 'NONE', #3080, 1000.000000000000000 ) ;
#7475 = ORIENTED_EDGE ( 'NONE', *, *, #1971, .F. ) ;
#7476 = EDGE_LOOP ( 'NONE', ( #4375, #3574, #6938, #3405 ) ) ;
#7477 = ORIENTED_EDGE ( 'NONE', *, *, #6643, .F. ) ;
#7478 = VERTEX_POINT ( 'NONE', #2150 ) ;
#7479 = VECTOR ( 'NONE', #893, 1000.000000000000000 ) ;
#7480 = DIRECTION ( 'NONE',  ( 1.000000000000000000, 0.000000000000000000, 0.000000000000000000 ) ) ;
#7481 = CARTESIAN_POINT ( 'NONE',  ( -4.000000000000000000, -33.63777638310832430, -3.000000000000000000 ) ) ;
#7482 = FILL_AREA_STYLE ('',( #7445 ) ) ;
#7483 = DIRECTION ( 'NONE',  ( -1.000000000000000000, 0.000000000000000000, 0.000000000000000000 ) ) ;
#7484 = ORIENTED_EDGE ( 'NONE', *, *, #3028, .T. ) ;
#7485 = AXIS2_PLACEMENT_3D ( 'NONE', #1301, #3758, #5977 ) ;
#7486 = ORIENTED_EDGE ( 'NONE', *, *, #938, .F. ) ;
#7487 = ORIENTED_EDGE ( 'NONE', *, *, #997, .F. ) ;
#7488 = DIRECTION ( 'NONE',  ( 1.000000000000000000, 0.000000000000000000, 0.000000000000000000 ) ) ;
#7489 = CARTESIAN_POINT ( 'NONE',  ( -207.8429183184020985, 119.9981648402869467, 10.00000000000000000 ) ) ;
#7490 = FACE_OUTER_BOUND ( 'NONE', #7081, .T. ) ;
#7491 = DIRECTION ( 'NONE',  ( 0.000000000000000000, 0.000000000000000000, 1.000000000000000000 ) ) ;
#7492 = VERTEX_POINT ( 'NONE', #1505 ) ;
#7493 = ADVANCED_FACE ( 'NONE', ( #7572 ), #6228, .T. ) ;
#7494 = DIRECTION ( 'NONE',  ( 0.000000000000000000, 0.000000000000000000, 1.000000000000000000 ) ) ;
#7495 = DIRECTION ( 'NONE',  ( -0.000000000000000000, -0.000000000000000000, 1.000000000000000000 ) ) ;
#7496 = VECTOR ( 'NONE', #1432, 1000.000000000000000 ) ;
#7497 = DIRECTION ( 'NONE',  ( 0.9412010056177179118, 0.3378471059875997051, 0.000000000000000000 ) ) ;
#7498 = CARTESIAN_POINT ( 'NONE',  ( -207.8429183184026670, 119.9981648402859378, -50.00000000000000000 ) ) ;
#7499 = EDGE_CURVE ( 'NONE', #4741, #7016, #4459, .T. ) ;
#7500 = ORIENTED_EDGE ( 'NONE', *, *, #4379, .F. ) ;
#7501 = VECTOR ( 'NONE', #1421, 1000.000000000000000 ) ;
#7502 = CARTESIAN_POINT ( 'NONE',  ( -3.499999999999996003, 0.000000000000000000, 0.000000000000000000 ) ) ;
#7503 = DIRECTION ( 'NONE',  ( 3.081487911019577365E-33, -2.775557561562891967E-17, -1.000000000000000000 ) ) ;
#7504 = DIRECTION ( 'NONE',  ( 0.000000000000000000, 1.224646799147359124E-16, 1.000000000000000000 ) ) ;
#7505 = CYLINDRICAL_SURFACE ( 'NONE', #6797, 5.250000000000000888 ) ;
#7506 = CARTESIAN_POINT ( 'NONE',  ( 4.494751301858288528, -36.47409643479112162, 0.000000000000000000 ) ) ;
#7507 = CONTEXT_DEPENDENT_SHAPE_REPRESENTATION ( #5363, #4783 ) ;
#7508 = AXIS2_PLACEMENT_3D ( 'NONE', #3555, #1752, #2970 ) ;
#7509 = FACE_OUTER_BOUND ( 'NONE', #6751, .T. ) ;
#7510 = VERTEX_POINT ( 'NONE', #6362 ) ;
#7511 = EDGE_LOOP ( 'NONE', ( #4004, #3991, #824, #7761 ) ) ;
#7512 = ORIENTED_EDGE ( 'NONE', *, *, #1278, .T. ) ;
#7513 = ADVANCED_FACE ( 'NONE', ( #3248, #6246 ), #4540, .T. ) ;
#7514 = AXIS2_PLACEMENT_3D ( 'NONE', #2743, #6255, #3888 ) ;
#7515 = VERTEX_POINT ( 'NONE', #2187 ) ;
#7516 = APPLICATION_CONTEXT ( 'automotive_design' ) ;
#7517 = DIRECTION ( 'NONE',  ( 1.000000000000000000, 0.000000000000000000, 0.000000000000000000 ) ) ;
#7518 = DIRECTION ( 'NONE',  ( 1.000000000000000000, 0.000000000000000000, 0.000000000000000000 ) ) ;
#7519 = DIRECTION ( 'NONE',  ( -1.000000000000000000, 0.000000000000000000, 0.000000000000000000 ) ) ;
#7520 = AXIS2_PLACEMENT_3D ( 'NONE', #3877, #2661, #7497 ) ;
#7521 = ORIENTED_EDGE ( 'NONE', *, *, #5287, .F. ) ;
#7522 = ORIENTED_EDGE ( 'NONE', *, *, #3093, .T. ) ;
#7523 = ORIENTED_EDGE ( 'NONE', *, *, #4625, .F. ) ;
#7524 = CIRCLE ( 'NONE', #2131, 5.250000000000000888 ) ;
#7525 = B_SPLINE_CURVE_WITH_KNOTS ( 'NONE', 3,
 ( #7164, #6454, #5985, #1045, #1729, #3456, #5865, #2910 ),
 .UNSPECIFIED., .F., .F.,
 ( 4, 2, 2, 4 ),
 ( 0.004673709593152153112, 0.005837709341827643401, 0.007001709090503134558, 0.009329708587854111668 ),
 .UNSPECIFIED. ) ;
#7526 = CARTESIAN_POINT ( 'NONE',  ( 0.000000000000000000, 0.000000000000000000, 20.00000000000000000 ) ) ;
#7527 =( LENGTH_UNIT ( ) NAMED_UNIT ( * ) SI_UNIT ( .MILLI., .METRE. ) );
#7528 = DIRECTION ( 'NONE',  ( 0.000000000000000000, 0.000000000000000000, 1.000000000000000000 ) ) ;
#7529 = DIRECTION ( 'NONE',  ( 0.000000000000000000, 0.000000000000000000, -1.000000000000000000 ) ) ;
#7530 = ORIENTED_EDGE ( 'NONE', *, *, #1968, .T. ) ;
#7531 = AXIS2_PLACEMENT_3D ( 'NONE', #479, #5291, #2932 ) ;
#7532 = ADVANCED_FACE ( 'NONE', ( #5168 ), #3287, .T. ) ;
#7533 = CARTESIAN_POINT ( 'NONE',  ( -3.660532965668821248, 7.124194613927619102, 4.997070872326744850E-15 ) ) ;
#7534 = DIRECTION ( 'NONE',  ( -1.000000000000000000, 0.000000000000000000, 0.000000000000000000 ) ) ;
#7535 = DIRECTION ( 'NONE',  ( -0.000000000000000000, -0.000000000000000000, 1.000000000000000000 ) ) ;
#7536 = FACE_OUTER_BOUND ( 'NONE', #5411, .T. ) ;
#7537 = VERTEX_POINT ( 'NONE', #6324 ) ;
#7538 = AXIS2_PLACEMENT_3D ( 'NONE', #995, #3410, #7624 ) ;
#7539 = ADVANCED_FACE ( 'NONE', ( #6949 ), #6838, .F. ) ;
#7540 = DIRECTION ( 'NONE',  ( -0.000000000000000000, -0.000000000000000000, 1.000000000000000000 ) ) ;
#7541 = DIRECTION ( 'NONE',  ( 0.000000000000000000, 0.000000000000000000, 1.000000000000000000 ) ) ;
#7542 = ADVANCED_FACE ( 'NONE', ( #4465 ), #908, .F. ) ;
#7543 = AXIS2_PLACEMENT_3D ( 'NONE', #458, #5947, #7756 ) ;
#7544 = EDGE_CURVE ( 'NONE', #5402, #154, #5350, .T. ) ;
#7545 = LINE ( 'NONE', #5221, #1559 ) ;
#7546 = DIRECTION ( 'NONE',  ( -0.000000000000000000, -0.000000000000000000, 1.000000000000000000 ) ) ;
#7547 = LINE ( 'NONE', #880, #95 ) ;
#7548 = ITEM_DEFINED_TRANSFORMATION ( 'NONE', 'NONE', #4975,  #7485 ) ;
#7549 = EDGE_CURVE ( 'NONE', #4996, #6340, #1585, .T. ) ;
#7550 = DIRECTION ( 'NONE',  ( 0.9412010056177179118, 0.3378471059875997051, 0.000000000000000000 ) ) ;
#7551 = VERTEX_POINT ( 'NONE', #6284 ) ;
#7552 = ORIENTED_EDGE ( 'NONE', *, *, #2848, .F. ) ;
#7553 = ORIENTED_EDGE ( 'NONE', *, *, #3937, .T. ) ;
#7554 = EDGE_CURVE ( 'NONE', #3827, #5742, #6102, .T. ) ;
#7555 = DIRECTION ( 'NONE',  ( 0.000000000000000000, 0.000000000000000000, 1.000000000000000000 ) ) ;
#7556 = DIRECTION ( 'NONE',  ( -1.000000000000000000, 0.000000000000000000, 0.000000000000000000 ) ) ;
#7557 = DIRECTION ( 'NONE',  ( -0.000000000000000000, -0.000000000000000000, -1.000000000000000000 ) ) ;
#7558 = DIRECTION ( 'NONE',  ( 0.000000000000000000, 0.000000000000000000, 1.000000000000000000 ) ) ;
#7559 = AXIS2_PLACEMENT_3D ( 'NONE', #435, #2931, #2850 ) ;
#7560 = DIRECTION ( 'NONE',  ( 0.000000000000000000, 0.000000000000000000, 1.000000000000000000 ) ) ;
#7561 = EDGE_LOOP ( 'NONE', ( #3949, #5859 ) ) ;
#7562 = ORIENTED_EDGE ( 'NONE', *, *, #5486, .T. ) ;
#7563 = AXIS2_PLACEMENT_3D ( 'NONE', #5677, #3906, #1457 ) ;
#7564 =( REPRESENTATION_RELATIONSHIP ('NONE','NONE', #1229, #637 ) REPRESENTATION_RELATIONSHIP_WITH_TRANSFORMATION ( #288 )SHAPE_REPRESENTATION_RELATIONSHIP( ) );
#7565 = ORIENTED_EDGE ( 'NONE', *, *, #1377, .T. ) ;
#7566 = DIRECTION ( 'NONE',  ( 1.000000000000000000, 0.000000000000000000, 0.000000000000000000 ) ) ;
#7567 = APPLICATION_PROTOCOL_DEFINITION ( 'draft international standard', 'automotive_design', 1998, #1220 ) ;
#7568 = DIRECTION ( 'NONE',  ( 0.000000000000000000, 0.000000000000000000, 1.000000000000000000 ) ) ;
#7569 = CYLINDRICAL_SURFACE ( 'NONE', #7468, 40.00000000000000711 ) ;
#7570 = ORIENTED_EDGE ( 'NONE', *, *, #5964, .F. ) ;
#7571 = CARTESIAN_POINT ( 'NONE',  ( -145.1064334105733451, -38.00161816111073421, 10.00000000000000000 ) ) ;
#7572 = FACE_OUTER_BOUND ( 'NONE', #374, .T. ) ;
#7573 = CARTESIAN_POINT ( 'NONE',  ( 4.000000000000004441, 6.928203230275507885, -4.700000000000000178 ) ) ;
#7574 = DIRECTION ( 'NONE',  ( 1.000000000000000000, 0.000000000000000000, 0.000000000000000000 ) ) ;
#7575 = AXIS2_PLACEMENT_3D ( 'NONE', #6210, #4505, #5096 ) ;
#7576 = ORIENTED_EDGE ( 'NONE', *, *, #794, .T. ) ;
#7577 = DIRECTION ( 'NONE',  ( -0.000000000000000000, -0.000000000000000000, 1.000000000000000000 ) ) ;
#7578 = CIRCLE ( 'NONE', #7463, 0.3000000000000016542 ) ;
#7579 = DIRECTION ( 'NONE',  ( 0.000000000000000000, 1.000000000000000000, 0.000000000000000000 ) ) ;
#7580 = DIRECTION ( 'NONE',  ( 1.000000000000000000, 0.000000000000000000, 0.000000000000000000 ) ) ;
#7581 = FACE_OUTER_BOUND ( 'NONE', #773, .T. ) ;
#7582 = CARTESIAN_POINT ( 'NONE',  ( -68.76644452187072432, 49.96174644486006855, -135.0000000000000000 ) ) ;
#7583 = DIRECTION ( 'NONE',  ( 1.000000000000000000, 0.000000000000000000, 0.000000000000000000 ) ) ;
#7584 = EDGE_CURVE ( 'NONE', #746, #1854, #3839, .T. ) ;
#7585 = EDGE_LOOP ( 'NONE', ( #7523, #6000, #1872, #1740 ) ) ;
#7586 = ORIENTED_EDGE ( 'NONE', *, *, #48, .F. ) ;
#7587 = CIRCLE ( 'NONE', #2692, 5.000000000000004441 ) ;
#7588 = ADVANCED_FACE ( 'NONE', ( #3445 ), #3294, .T. ) ;
#7589 = EDGE_LOOP ( 'NONE', ( #7252, #3752 ) ) ;
#7590 = ADVANCED_FACE ( 'NONE', ( #7037 ), #7663, .F. ) ;
#7591 = ORIENTED_EDGE ( 'NONE', *, *, #6796, .F. ) ;
#7592 = PLANE ( 'NONE',  #916 ) ;
#7593 = CARTESIAN_POINT ( 'NONE',  ( 29.99999999999999289, 0.000000000000000000, -79.99999999999995737 ) ) ;
#7594 = DIRECTION ( 'NONE',  ( 0.000000000000000000, 0.000000000000000000, 1.000000000000000000 ) ) ;
#7595 = DIRECTION ( 'NONE',  ( 0.000000000000000000, 0.000000000000000000, 1.000000000000000000 ) ) ;
#7596 = AXIS2_PLACEMENT_3D ( 'NONE', #6510, #549, #5367 ) ;
#7597 = PRESENTATION_STYLE_ASSIGNMENT (( #4125 ) ) ;
#7598 = ADVANCED_FACE ( 'NONE', ( #1513, #2859, #918 ), #956, .T. ) ;
#7599 = VERTEX_POINT ( 'NONE', #5813 ) ;
#7600 = EDGE_LOOP ( 'NONE', ( #195, #7192, #6894, #4057 ) ) ;
#7601 = AXIS2_PLACEMENT_3D ( 'NONE', #262, #5749, #7519 ) ;
#7602 = AXIS2_PLACEMENT_3D ( 'NONE', #318, #5130, #5211 ) ;
#7603 = VERTEX_POINT ( 'NONE', #3919 ) ;
#7604 = DIRECTION ( 'NONE',  ( -0.000000000000000000, -0.000000000000000000, -1.000000000000000000 ) ) ;
#7605 = PRODUCT_CONTEXT ( 'NONE', #405, 'mechanical' ) ;
#7606 = CARTESIAN_POINT ( 'NONE',  ( -150.0000000000000568, 0.000000000000000000, 0.000000000000000000 ) ) ;
#7607 = AXIS2_PLACEMENT_3D ( 'NONE', #4245, #6657, #1247 ) ;
#7608 =( GEOMETRIC_REPRESENTATION_CONTEXT ( 3 ) GLOBAL_UNCERTAINTY_ASSIGNED_CONTEXT ( ( #6031 ) ) GLOBAL_UNIT_ASSIGNED_CONTEXT ( ( #7527, #4378, #5604 ) ) REPRESENTATION_CONTEXT ( 'NONE', 'WORKASPACE' ) );
#7609 = LINE ( 'NONE', #4021, #6718 ) ;
#7610 = ORIENTED_EDGE ( 'NONE', *, *, #1869, .F. ) ;
#7611 = ORIENTED_EDGE ( 'NONE', *, *, #6303, .T. ) ;
#7612 = AXIS2_PLACEMENT_3D ( 'NONE', #3726, #4828, #6135 ) ;
#7613 = FACE_OUTER_BOUND ( 'NONE', #292, .T. ) ;
#7614 = CARTESIAN_POINT ( 'NONE',  ( -150.0000000000000568, 0.000000000000000000, 10.00000000000000000 ) ) ;
#7615 = DIRECTION ( 'NONE',  ( 0.7071067811865474617, 0.000000000000000000, 0.7071067811865474617 ) ) ;
#7616 = CARTESIAN_POINT ( 'NONE',  ( 0.000000000000000000, 0.000000000000000000, 0.000000000000000000 ) ) ;
#7617 = VERTEX_POINT ( 'NONE', #2195 ) ;
#7618 = AXIS2_PLACEMENT_3D ( 'NONE', #4281, #582, #6100 ) ;
#7619 = VERTEX_POINT ( 'NONE', #6923 ) ;
#7620 =( REPRESENTATION_RELATIONSHIP ('NONE','NONE', #1229, #1433 ) REPRESENTATION_RELATIONSHIP_WITH_TRANSFORMATION ( #2983 )SHAPE_REPRESENTATION_RELATIONSHIP( ) );
#7621 = CARTESIAN_POINT ( 'NONE',  ( -5.690023276062397883, -5.952467836904158816, -0.1306530452038143220 ) ) ;
#7622 = DIRECTION ( 'NONE',  ( 0.000000000000000000, 0.000000000000000000, 1.000000000000000000 ) ) ;
#7623 = DIRECTION ( 'NONE',  ( 0.000000000000000000, 1.000000000000000000, -1.224646799147353207E-16 ) ) ;
#7624 = DIRECTION ( 'NONE',  ( -1.000000000000000000, 0.000000000000000000, 0.000000000000000000 ) ) ;
#7625 = DIRECTION ( 'NONE',  ( 1.000000000000000000, 0.000000000000000000, 0.000000000000000000 ) ) ;
#7626 = CARTESIAN_POINT ( 'NONE',  ( -1.728922298134113098E-15, 8.513302795252935035E-16, 13.00000000000000178 ) ) ;
#7627 = ORIENTED_EDGE ( 'NONE', *, *, #5103, .F. ) ;
#7628 = VECTOR ( 'NONE', #1761, 1000.000000000000000 ) ;
#7629 = VERTEX_POINT ( 'NONE', #877 ) ;
#7630 = ORIENTED_EDGE ( 'NONE', *, *, #1372, .F. ) ;
#7631 = PRODUCT_RELATED_PRODUCT_CATEGORY ( 'part', '', ( #131 ) ) ;
#7632 = DIRECTION ( 'NONE',  ( -0.000000000000000000, -0.000000000000000000, 1.000000000000000000 ) ) ;
#7633 = AXIS2_PLACEMENT_3D ( 'NONE', #1873, #3136, #4267 ) ;
#7634 = DIRECTION ( 'NONE',  ( -1.000000000000000000, 0.000000000000000000, 0.000000000000000000 ) ) ;
#7635 = LINE ( 'NONE', #497, #5881 ) ;
#7636 = SHAPE_REPRESENTATION_RELATIONSHIP ( 'NONE' , 'NONE' ,  #420, #1052 ) ;
#7637 = DIRECTION ( 'NONE',  ( 1.000000000000000000, 0.000000000000000000, 0.000000000000000000 ) ) ;
#7638 = DIRECTION ( 'NONE',  ( 1.000000000000000000, 0.000000000000000000, 0.000000000000000000 ) ) ;
#7639 = ORIENTED_EDGE ( 'NONE', *, *, #2081, .T. ) ;
#7640 = CIRCLE ( 'NONE', #2242, 8.000000000000000000 ) ;
#7641 = EDGE_LOOP ( 'NONE', ( #2294, #594 ) ) ;
#7642 = VERTEX_POINT ( 'NONE', #1552 ) ;
#7643 = DIRECTION ( 'NONE',  ( 0.000000000000000000, 0.000000000000000000, 1.000000000000000000 ) ) ;
#7644 = EDGE_CURVE ( 'NONE', #1102, #6819, #5692, .T. ) ;
#7645 = TOROIDAL_SURFACE ( 'NONE', #1739, 33.75000000000000000, 2.250000000000000444 ) ;
#7646 = DIRECTION ( 'NONE',  ( 0.000000000000000000, 0.000000000000000000, 1.000000000000000000 ) ) ;
#7647 = EDGE_CURVE ( 'NONE', #1532, #2100, #2782, .T. ) ;
#7648 = CARTESIAN_POINT ( 'NONE',  ( 21.01644452187054313, 80.83980388508807380, 10.00000000000000000 ) ) ;
#7649 = ORIENTED_EDGE ( 'NONE', *, *, #7217, .F. ) ;
#7650 = CIRCLE ( 'NONE', #6399, 40.00000000000000000 ) ;
#7651 = ADVANCED_FACE ( 'NONE', ( #3885 ), #1476, .T. ) ;
#7652 = CARTESIAN_POINT ( 'NONE',  ( 213.0929183184020985, 119.9981648402868331, -120.0000000000000000 ) ) ;
#7653 = CARTESIAN_POINT ( 'NONE',  ( 0.000000000000000000, 0.000000000000000000, -50.00000000000000000 ) ) ;
#7654 = LINE ( 'NONE', #6403, #4889 ) ;
#7655 = VECTOR ( 'NONE', #6757, 1000.000000000000000 ) ;
#7656 = CARTESIAN_POINT ( 'NONE',  ( 0.5700000000000001732, -28.49429942988597020, -3.000000000000000000 ) ) ;
#7657 = EDGE_CURVE ( 'NONE', #913, #5664, #298, .T. ) ;
#7658 = ORIENTED_EDGE ( 'NONE', *, *, #2357, .T. ) ;
#7659 = ORIENTED_EDGE ( 'NONE', *, *, #215, .F. ) ;
#7660 = CIRCLE ( 'NONE', #7034, 5.250000000000004441 ) ;
#7661 = DIRECTION ( 'NONE',  ( 1.000000000000000000, 0.000000000000000000, 0.000000000000000000 ) ) ;
#7662 = CARTESIAN_POINT ( 'NONE',  ( 5.238334947888644955, -36.57199107895616663, -3.000000000000000000 ) ) ;
#7663 = CYLINDRICAL_SURFACE ( 'NONE', #7363, 5.249999999999992006 ) ;
#7664 = FACE_OUTER_BOUND ( 'NONE', #2976, .T. ) ;
#7665 = DIRECTION ( 'NONE',  ( -0.000000000000000000, -0.000000000000000000, -1.000000000000000000 ) ) ;
#7666 = AXIS2_PLACEMENT_3D ( 'NONE', #2551, #902, #4574 ) ;
#7667 = DIRECTION ( 'NONE',  ( 0.000000000000000000, 0.000000000000000000, 1.000000000000000000 ) ) ;
#7668 = ORIENTED_EDGE ( 'NONE', *, *, #5282, .T. ) ;
#7669 =( REPRESENTATION_RELATIONSHIP ('NONE','NONE', #1229, #2051 ) REPRESENTATION_RELATIONSHIP_WITH_TRANSFORMATION ( #7548 )SHAPE_REPRESENTATION_RELATIONSHIP( ) );
#7670 = ORIENTED_EDGE ( 'NONE', *, *, #3357, .T. ) ;
#7671 = ORIENTED_EDGE ( 'NONE', *, *, #2025, .T. ) ;
#7672 = CIRCLE ( 'NONE', #6805, 10.00000000000000178 ) ;
#7673 = FACE_OUTER_BOUND ( 'NONE', #7382, .T. ) ;
#7674 = DIRECTION ( 'NONE',  ( 1.000000000000000000, 0.000000000000000000, 0.000000000000000000 ) ) ;
#7675 = CARTESIAN_POINT ( 'NONE',  ( 0.000000000000000000, 0.000000000000000000, -3.000000000000000000 ) ) ;
#7676 = DIRECTION ( 'NONE',  ( 0.000000000000000000, 0.000000000000000000, 1.000000000000000000 ) ) ;
#7677 = LINE ( 'NONE', #6623, #2271 ) ;
#7678 = AXIS2_PLACEMENT_3D ( 'NONE', #5476, #3118, #111 ) ;
#7679 = ORIENTED_EDGE ( 'NONE', *, *, #7644, .F. ) ;
#7680 = VERTEX_POINT ( 'NONE', #5141 ) ;
#7681 = ORIENTED_EDGE ( 'NONE', *, *, #4317, .F. ) ;
#7682 = AXIS2_PLACEMENT_3D ( 'NONE', #6830, #4534, #827 ) ;
#7683 = CARTESIAN_POINT ( 'NONE',  ( 3.499999999999996003, 0.000000000000000000, 0.000000000000000000 ) ) ;
#7684 = FACE_OUTER_BOUND ( 'NONE', #6096, .T. ) ;
#7685 = SURFACE_STYLE_USAGE ( .BOTH. , #1059 ) ;
#7686 = DIRECTION ( 'NONE',  ( -1.000000000000000000, 1.224646799147352961E-16, 0.000000000000000000 ) ) ;
#7687 = CARTESIAN_POINT ( 'NONE',  ( -26.82422866010496776, -9.628642520646595315, -122.9999999999999716 ) ) ;
#7688 = EDGE_CURVE ( 'NONE', #1428, #7617, #5718, .T. ) ;
#7689 = VERTEX_POINT ( 'NONE', #3332 ) ;
#7690 = AXIS2_PLACEMENT_3D ( 'NONE', #267, #5081, #2104 ) ;
#7691 = EDGE_CURVE ( 'NONE', #7044, #5950, #4336, .T. ) ;
#7692 = EDGE_CURVE ( 'NONE', #3552, #1298, #1950, .T. ) ;
#7693 = EDGE_CURVE ( 'NONE', #7603, #1043, #6292, .T. ) ;
#7694 = CARTESIAN_POINT ( 'NONE',  ( -39.64284999284935651, -144.6666666666667140, 0.000000000000000000 ) ) ;
#7695 = CYLINDRICAL_SURFACE ( 'NONE', #3284, 28.50000000000000355 ) ;
#7696 = AXIS2_PLACEMENT_3D ( 'NONE', #6267, #225, #1488 ) ;
#7697 = DIRECTION ( 'NONE',  ( -0.000000000000000000, -0.000000000000000000, 1.000000000000000000 ) ) ;
#7698 = CARTESIAN_POINT ( 'NONE',  ( 0.000000000000000000, 0.000000000000000000, 20.00000000000000000 ) ) ;
#7699 = ORIENTED_EDGE ( 'NONE', *, *, #1971, .T. ) ;
#7700 = EDGE_LOOP ( 'NONE', ( #6136, #5109 ) ) ;
#7701 = EDGE_CURVE ( 'NONE', #2888, #5846, #7545, .T. ) ;
#7702 = CIRCLE ( 'NONE', #23, 5.250000000000004441 ) ;
#7703 = CARTESIAN_POINT ( 'NONE',  ( 0.000000000000000000, 0.000000000000000000, 9.480888224575629408 ) ) ;
#7704 = SURFACE_SIDE_STYLE ('',( #5771 ) ) ;
#7705 = DIRECTION ( 'NONE',  ( -0.000000000000000000, -0.000000000000000000, 1.000000000000000000 ) ) ;
#7706 = DIRECTION ( 'NONE',  ( 0.000000000000000000, 0.000000000000000000, 1.000000000000000000 ) ) ;
#7707 = CYLINDRICAL_SURFACE ( 'NONE', #1193, 8.000000000000000000 ) ;
#7708 = ORIENTED_EDGE ( 'NONE', *, *, #7127, .T. ) ;
#7709 = ORIENTED_EDGE ( 'NONE', *, *, #7584, .F. ) ;
#7710 = EDGE_LOOP ( 'NONE', ( #2967, #899 ) ) ;
#7711 = FACE_OUTER_BOUND ( 'NONE', #775, .T. ) ;
#7712 = CARTESIAN_POINT ( 'NONE',  ( -5.134781488891348999E-13, 239.9963296805737230, -120.0000000000000000 ) ) ;
#7713 = FACE_OUTER_BOUND ( 'NONE', #1795, .T. ) ;
#7714 = CARTESIAN_POINT ( 'NONE',  ( 26.26644452186938850, 80.83980388508842907, 14.69999999999999929 ) ) ;
#7715 = CARTESIAN_POINT ( 'NONE',  ( -3.199999999999996181, 0.000000000000000000, 0.000000000000000000 ) ) ;
#7716 = CARTESIAN_POINT ( 'NONE',  ( 90.25000000000001421, 9.720002580593245511E-13, 10.00000000000000000 ) ) ;
#7717 = CARTESIAN_POINT ( 'NONE',  ( -8.000000000000000000, 0.000000000000000000, 0.000000000000000000 ) ) ;
#7718 = EDGE_LOOP ( 'NONE', ( #313, #563 ) ) ;
#7719 = EDGE_LOOP ( 'NONE', ( #7173, #4373, #6761, #5602, #493, #3156 ) ) ;
#7720 = EDGE_LOOP ( 'NONE', ( #5147, #2101, #1305, #3781, #5875, #3894, #4983, #4333, #678, #5217, #5452, #6272, #5295, #4673, #4781, #1268 ) ) ;
#7721 = CIRCLE ( 'NONE', #2066, 40.00000000000001421 ) ;
#7722 = CARTESIAN_POINT ( 'NONE',  ( -8.000000000000000000, 1.572549600175617401, -4.631055444744868410 ) ) ;
#7723 = DIRECTION ( 'NONE',  ( 0.000000000000000000, 0.000000000000000000, 1.000000000000000000 ) ) ;
#7724 = DIRECTION ( 'NONE',  ( -0.000000000000000000, -0.000000000000000000, -1.000000000000000000 ) ) ;
#7725 = SHAPE_REPRESENTATION ( 'stud long', ( #7485 ), #6239 ) ;
#7726 = VECTOR ( 'NONE', #7646, 1000.000000000000000 ) ;
#7727 = ORIENTED_EDGE ( 'NONE', *, *, #610, .F. ) ;
#7728 = DIRECTION ( 'NONE',  ( 0.9845265360683707057, 0.1752355551171480841, 0.000000000000000000 ) ) ;
#7729 = DIRECTION ( 'NONE',  ( 0.000000000000000000, 0.000000000000000000, 1.000000000000000000 ) ) ;
#7730 = CIRCLE ( 'NONE', #4334, 5.249999999999995559 ) ;
#7731 = AXIS2_PLACEMENT_3D ( 'NONE', #2704, #2819, #6331 ) ;
#7732 = DIRECTION ( 'NONE',  ( 1.000000000000000000, 0.000000000000000000, 0.000000000000000000 ) ) ;
#7733 = DIRECTION ( 'NONE',  ( -0.000000000000000000, -0.000000000000000000, 1.000000000000000000 ) ) ;
#7734 = ORIENTED_EDGE ( 'NONE', *, *, #7448, .T. ) ;
#7735 = EDGE_CURVE ( 'NONE', #5401, #4002, #3580, .T. ) ;
#7736 = EDGE_LOOP ( 'NONE', ( #7552, #5498, #4690, #5412 ) ) ;
#7737 =( GEOMETRIC_REPRESENTATION_CONTEXT ( 3 ) GLOBAL_UNCERTAINTY_ASSIGNED_CONTEXT ( ( #4881 ) ) GLOBAL_UNIT_ASSIGNED_CONTEXT ( ( #5796, #1016, #6466 ) ) REPRESENTATION_CONTEXT ( 'NONE', 'WORKASPACE' ) );
#7738 = ORIENTED_EDGE ( 'NONE', *, *, #215, .T. ) ;
#7739 = DIRECTION ( 'NONE',  ( 0.000000000000000000, 0.000000000000000000, -1.000000000000000000 ) ) ;
#7740 = CARTESIAN_POINT ( 'NONE',  ( 8.000000000000000000, 3.871967595402126872, -0.4989386132324573064 ) ) ;
#7741 = FACE_OUTER_BOUND ( 'NONE', #3240, .T. ) ;
#7742 = CARTESIAN_POINT ( 'NONE',  ( 3.500000000000006661, 0.000000000000000000, 0.000000000000000000 ) ) ;
#7743 = ITEM_DEFINED_TRANSFORMATION ( 'NONE', 'NONE', #1843,  #7485 ) ;
#7744 = ADVANCED_FACE ( 'NONE', ( #4547 ), #3409, .T. ) ;
#7745 =( GEOMETRIC_REPRESENTATION_CONTEXT ( 3 ) GLOBAL_UNCERTAINTY_ASSIGNED_CONTEXT ( ( #4285 ) ) GLOBAL_UNIT_ASSIGNED_CONTEXT ( ( #3462, #2872, #6973 ) ) REPRESENTATION_CONTEXT ( 'NONE', 'WORKASPACE' ) );
#7746 = CARTESIAN_POINT ( 'NONE',  ( 0.000000000000000000, 0.000000000000000000, -82.99999999999995737 ) ) ;
#7747 = EDGE_LOOP ( 'NONE', ( #2790, #7294 ) ) ;
#7748 = ORIENTED_EDGE ( 'NONE', *, *, #3649, .F. ) ;
#7749 = CARTESIAN_POINT ( 'NONE',  ( -4.681481898397001018, 6.534749472788146996, -4.700000000000005507 ) ) ;
#7750 = EDGE_CURVE ( 'NONE', #219, #3671, #4463, .T. ) ;
#7751 = DIRECTION ( 'NONE',  ( 1.000000000000000000, 0.000000000000000000, 0.000000000000000000 ) ) ;
#7752 = LINE ( 'NONE', #413, #4114 ) ;
#7753 = CARTESIAN_POINT ( 'NONE',  ( -1.728922298134113098E-15, 8.513302795252935035E-16, 10.00000000000000000 ) ) ;
#7754 = CIRCLE ( 'NONE', #5618, 4.171999999999995268 ) ;
#7755 = CARTESIAN_POINT ( 'NONE',  ( -3.499999999999996003, 0.000000000000000000, 0.000000000000000000 ) ) ;
#7756 = DIRECTION ( 'NONE',  ( 0.9845265360683707057, 0.1752355551171480841, 0.000000000000000000 ) ) ;
#7757 = ADVANCED_FACE ( 'NONE', ( #526 ), #4300, .F. ) ;
#7758 = EDGE_LOOP ( 'NONE', ( #4805, #6452 ) ) ;
#7759 = VERTEX_POINT ( 'NONE', #121 ) ;
#7760 = VECTOR ( 'NONE', #2549, 1000.000000000000114 ) ;
#7761 = ORIENTED_EDGE ( 'NONE', *, *, #1981, .T. ) ;
#7762 = CARTESIAN_POINT ( 'NONE',  ( -8.000000000000000000, 0.7809653281576043327, -4.700000000000000178 ) ) ;
#7763 = EDGE_LOOP ( 'NONE', ( #3339, #1627, #1383, #7457, #6582, #2052, #5896, #1495 ) ) ;
#7764 = NEXT_ASSEMBLY_USAGE_OCCURRENCE ( 'NAUO1', ' ', ' ', #3786, #3590, $ ) ;
#7765 = NEXT_ASSEMBLY_USAGE_OCCURRENCE ( 'NAUO2', ' ', ' ', #3786, #1223, $ ) ;
#7766 = NEXT_ASSEMBLY_USAGE_OCCURRENCE ( 'NAUO3', ' ', ' ', #3786, #6003, $ ) ;
#7767 = NEXT_ASSEMBLY_USAGE_OCCURRENCE ( 'NAUO4', ' ', ' ', #3786, #6478, $ ) ;
#7768 = NEXT_ASSEMBLY_USAGE_OCCURRENCE ( 'NAUO5', ' ', ' ', #3786, #6722, $ ) ;
#7769 = NEXT_ASSEMBLY_USAGE_OCCURRENCE ( 'NAUO6', ' ', ' ', #3786, #3590, $ ) ;
#7770 = NEXT_ASSEMBLY_USAGE_OCCURRENCE ( 'NAUO7', ' ', ' ', #3786, #1223, $ ) ;
#7771 = NEXT_ASSEMBLY_USAGE_OCCURRENCE ( 'NAUO8', ' ', ' ', #3786, #7394, $ ) ;
#7772 = NEXT_ASSEMBLY_USAGE_OCCURRENCE ( 'NAUO9', ' ', ' ', #3786, #7394, $ ) ;
#7773 = NEXT_ASSEMBLY_USAGE_OCCURRENCE ( 'NAUO10', ' ', ' ', #3786, #7394, $ ) ;
#7774 = NEXT_ASSEMBLY_USAGE_OCCURRENCE ( 'NAUO11', ' ', ' ', #3786, #7394, $ ) ;
#7775 = NEXT_ASSEMBLY_USAGE_OCCURRENCE ( 'NAUO12', ' ', ' ', #3786, #7394, $ ) ;
#7776 = NEXT_ASSEMBLY_USAGE_OCCURRENCE ( 'NAUO13', ' ', ' ', #3786, #6003, $ ) ;
#7777 = NEXT_ASSEMBLY_USAGE_OCCURRENCE ( 'NAUO14', ' ', ' ', #3786, #6003, $ ) ;
#7778 = NEXT_ASSEMBLY_USAGE_OCCURRENCE ( 'NAUO15', ' ', ' ', #3786, #6003, $ ) ;
#7779 = NEXT_ASSEMBLY_USAGE_OCCURRENCE ( 'NAUO16', ' ', ' ', #3786, #7394, $ ) ;
#7780 = NEXT_ASSEMBLY_USAGE_OCCURRENCE ( 'NAUO17', ' ', ' ', #3786, #7394, $ ) ;
#7781 = NEXT_ASSEMBLY_USAGE_OCCURRENCE ( 'NAUO18', ' ', ' ', #3786, #7394, $ ) ;
#7782 = NEXT_ASSEMBLY_USAGE_OCCURRENCE ( 'NAUO19', ' ', ' ', #3786, #302, $ ) ;
#7783 = NEXT_ASSEMBLY_USAGE_OCCURRENCE ( 'NAUO20', ' ', ' ', #3786, #7394, $ ) ;
#7784 = NEXT_ASSEMBLY_USAGE_OCCURRENCE ( 'NAUO21', ' ', ' ', #3786, #7394, $ ) ;
#7785 = NEXT_ASSEMBLY_USAGE_OCCURRENCE ( 'NAUO22', ' ', ' ', #3786, #4161, $ ) ;
#7786 = NEXT_ASSEMBLY_USAGE_OCCURRENCE ( 'NAUO23', ' ', ' ', #3786, #7059, $ ) ;
#7787 = NEXT_ASSEMBLY_USAGE_OCCURRENCE ( 'NAUO24', ' ', ' ', #3786, #7059, $ ) ;
#7788 = NEXT_ASSEMBLY_USAGE_OCCURRENCE ( 'NAUO25', ' ', ' ', #3786, #4161, $ ) ;
#7789 = NEXT_ASSEMBLY_USAGE_OCCURRENCE ( 'NAUO26', ' ', ' ', #3786, #4161, $ ) ;
#7790 = NEXT_ASSEMBLY_USAGE_OCCURRENCE ( 'NAUO27', ' ', ' ', #3786, #7394, $ ) ;
#7791 = NEXT_ASSEMBLY_USAGE_OCCURRENCE ( 'NAUO28', ' ', ' ', #3786, #7394, $ ) ;
#7792 = NEXT_ASSEMBLY_USAGE_OCCURRENCE ( 'NAUO29', ' ', ' ', #3786, #7394, $ ) ;
#7793 = NEXT_ASSEMBLY_USAGE_OCCURRENCE ( 'NAUO30', ' ', ' ', #3786, #7394, $ ) ;
#7794 = NEXT_ASSEMBLY_USAGE_OCCURRENCE ( 'NAUO31', ' ', ' ', #3786, #7394, $ ) ;
#7795 = NEXT_ASSEMBLY_USAGE_OCCURRENCE ( 'NAUO32', ' ', ' ', #3786, #302, $ ) ;
#7796 = NEXT_ASSEMBLY_USAGE_OCCURRENCE ( 'NAUO33', ' ', ' ', #3786, #302, $ ) ;
#7797 = NEXT_ASSEMBLY_USAGE_OCCURRENCE ( 'NAUO34', ' ', ' ', #3786, #302, $ ) ;
#7798 = NEXT_ASSEMBLY_USAGE_OCCURRENCE ( 'NAUO35', ' ', ' ', #3786, #302, $ ) ;
#7799 = NEXT_ASSEMBLY_USAGE_OCCURRENCE ( 'NAUO36', ' ', ' ', #3786, #7394, $ ) ;
#7800 = NEXT_ASSEMBLY_USAGE_OCCURRENCE ( 'NAUO37', ' ', ' ', #3786, #7394, $ ) ;
#7801 = NEXT_ASSEMBLY_USAGE_OCCURRENCE ( 'NAUO38', ' ', ' ', #3786, #7394, $ ) ;
#7802 = NEXT_ASSEMBLY_USAGE_OCCURRENCE ( 'NAUO39', ' ', ' ', #3786, #7394, $ ) ;
#7803=COLOUR_RGB('Dark Blue',0.08,0.2,0.34);
#7804=FILL_AREA_STYLE_COLOUR('',#7803);
#7805=FILL_AREA_STYLE('',(#7804));
#7806=SURFACE_STYLE_FILL_AREA(#7805);
#7807=SURFACE_SIDE_STYLE('',(#7806));
#7808=SURFACE_STYLE_USAGE(.BOTH.,#7807);
#7809=PRESENTATION_STYLE_ASSIGNMENT((#7808));
#7810=COLOUR_RGB('Light Blue',0.38,0.62,0.78);
#7811=FILL_AREA_STYLE_COLOUR('',#7810);
#7812=FILL_AREA_STYLE('',(#7811));
#7813=SURFACE_STYLE_FILL_AREA(#7812);
#7814=SURFACE_SIDE_STYLE('',(#7813));
#7815=SURFACE_STYLE_USAGE(.BOTH.,#7814);
#7816=PRESENTATION_STYLE_ASSIGNMENT((#7815));
#7817=COLOUR_RGB('Sky Blue',0.24,0.69,0.87);
#7818=FILL_AREA_STYLE_COLOUR('',#7817);
#7819=FILL_AREA_STYLE('',(#7818));
#7820=SURFACE_STYLE_FILL_AREA(#7819);
#7821=SURFACE_SIDE_STYLE('',(#7820));
#7822=SURFACE_STYLE_USAGE(.BOTH.,#7821);
#7823=PRESENTATION_STYLE_ASSIGNMENT((#7822));
#7824=COLOUR_RGB('Grey',0.48,0.52,0.57);
#7825=FILL_AREA_STYLE_COLOUR('',#7824);
#7826=FILL_AREA_STYLE('',(#7825));
#7827=SURFACE_STYLE_FILL_AREA(#7826);
#7828=SURFACE_SIDE_STYLE('',(#7827));
#7829=SURFACE_STYLE_USAGE(.BOTH.,#7828);
#7830=PRESENTATION_STYLE_ASSIGNMENT((#7829));
#7831=COLOUR_RGB('Black',0.12,0.14,0.17);
#7832=FILL_AREA_STYLE_COLOUR('',#7831);
#7833=FILL_AREA_STYLE('',(#7832));
#7834=SURFACE_STYLE_FILL_AREA(#7833);
#7835=SURFACE_SIDE_STYLE('',(#7834));
#7836=SURFACE_STYLE_USAGE(.BOTH.,#7835);
#7837=PRESENTATION_STYLE_ASSIGNMENT((#7836));
#7838=COLOUR_RGB('Off White',0.89,0.88,0.83);
#7839=FILL_AREA_STYLE_COLOUR('',#7838);
#7840=FILL_AREA_STYLE('',(#7839));
#7841=SURFACE_STYLE_FILL_AREA(#7840);
#7842=SURFACE_SIDE_STYLE('',(#7841));
#7843=SURFACE_STYLE_USAGE(.BOTH.,#7842);
#7844=PRESENTATION_STYLE_ASSIGNMENT((#7843));
ENDSEC;
END-ISO-10303-21;
